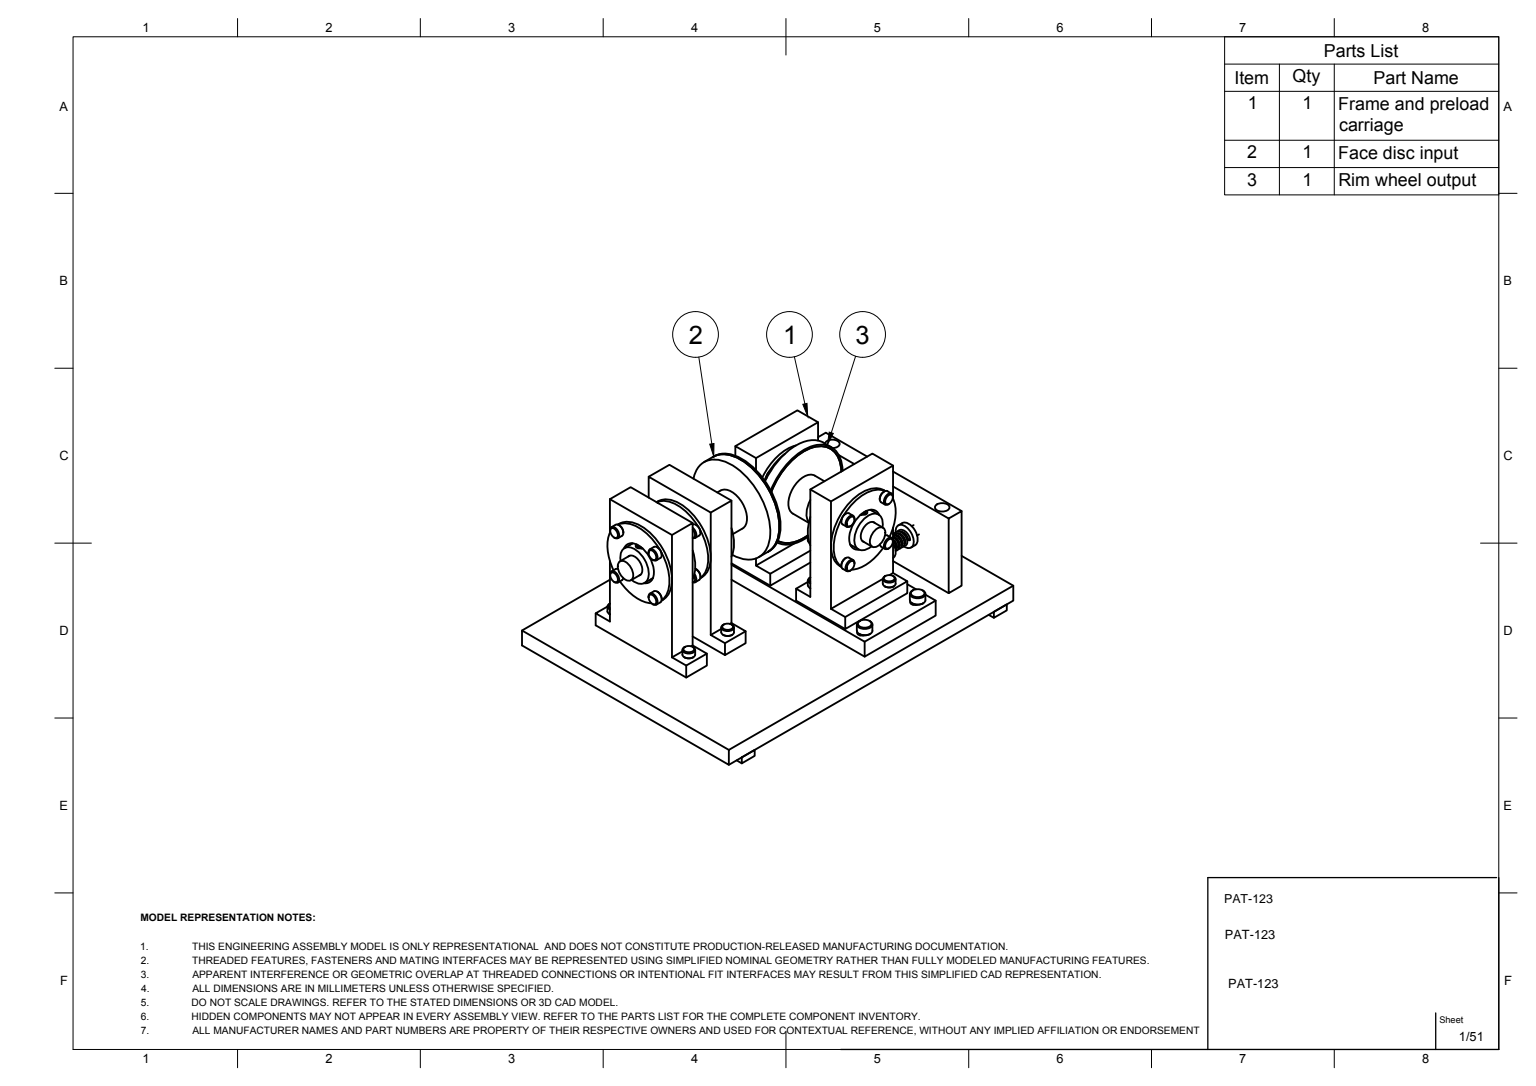
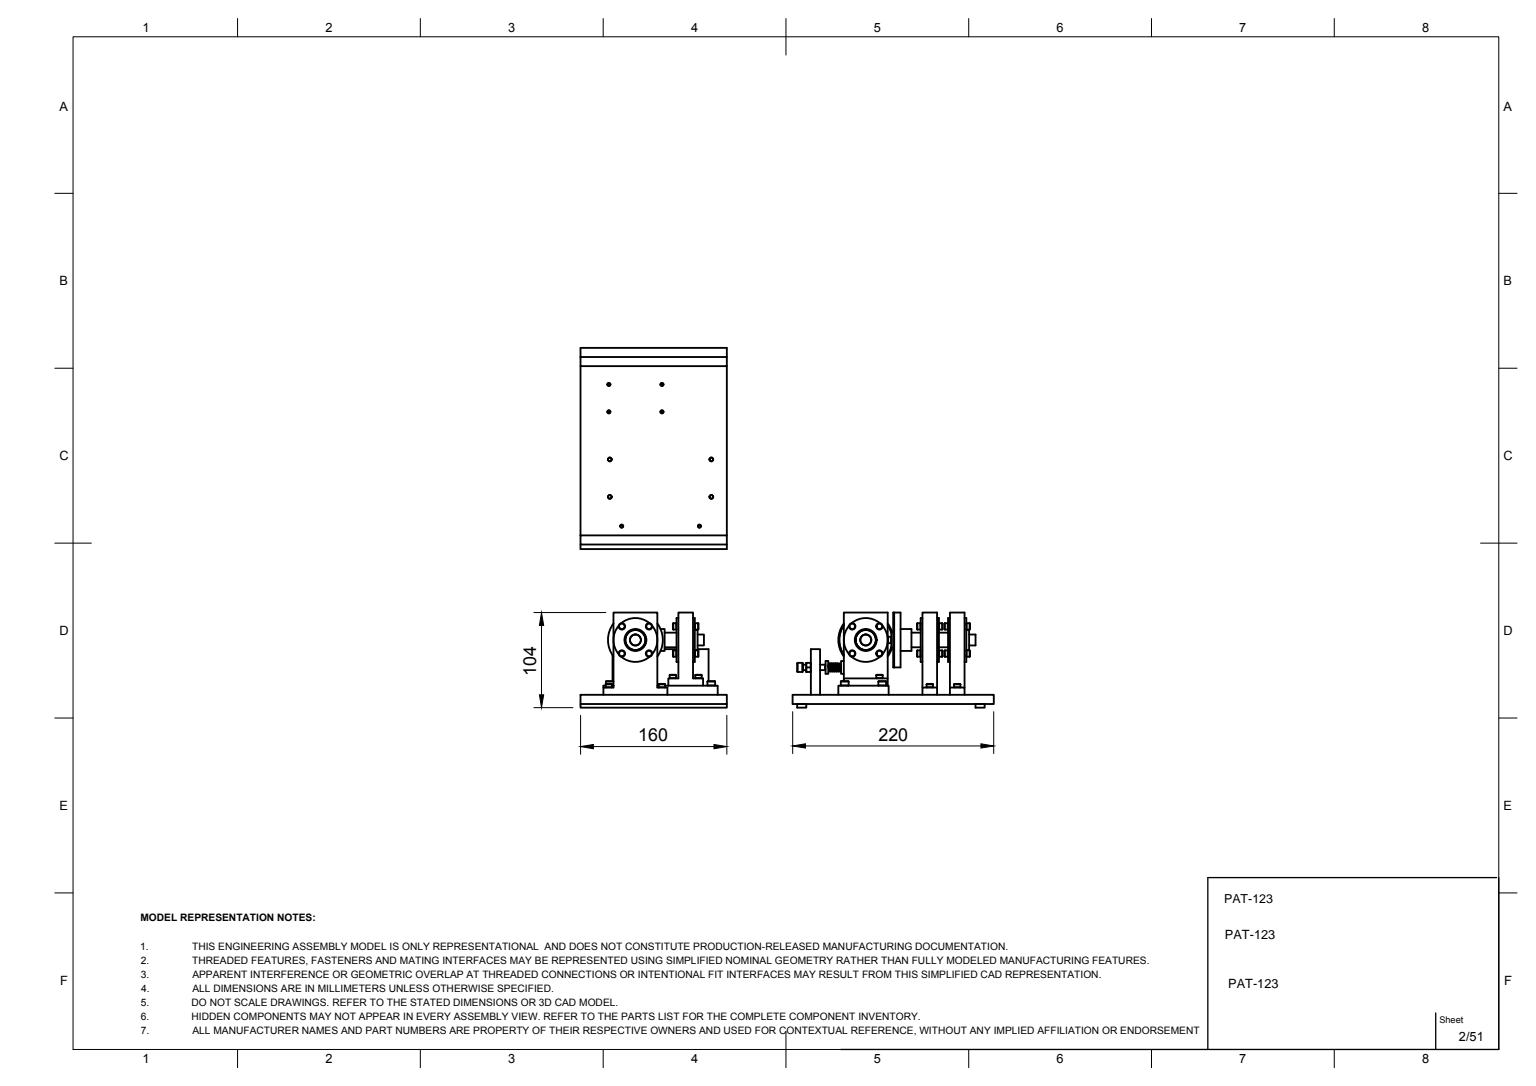
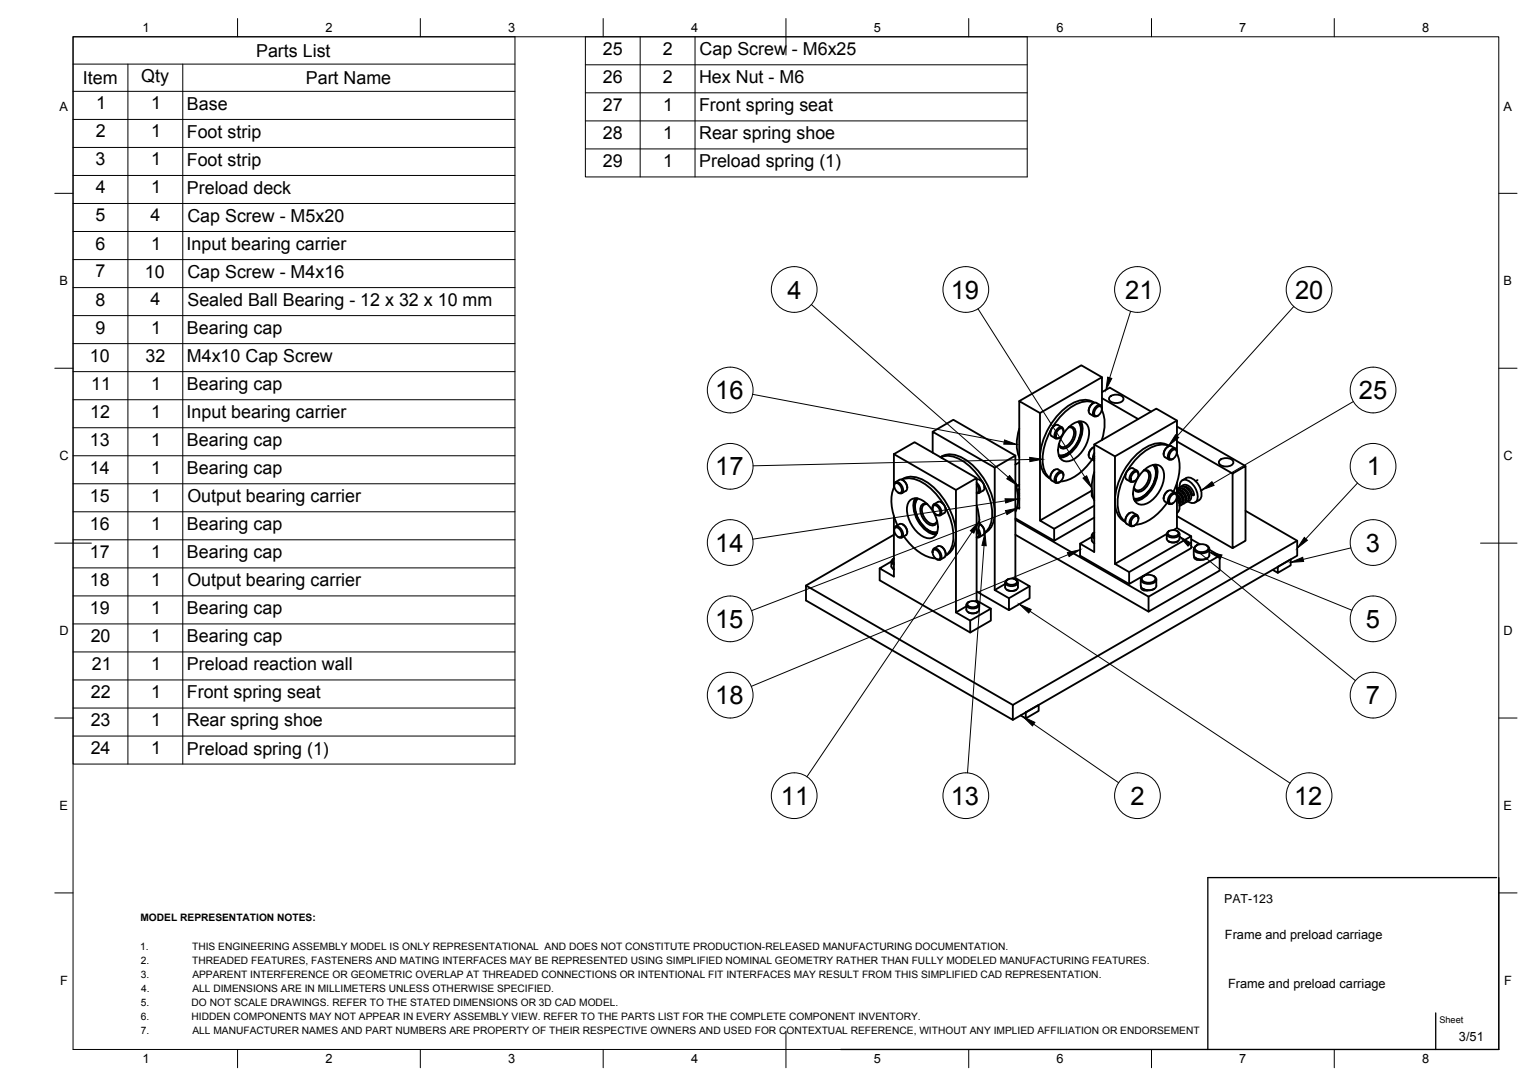
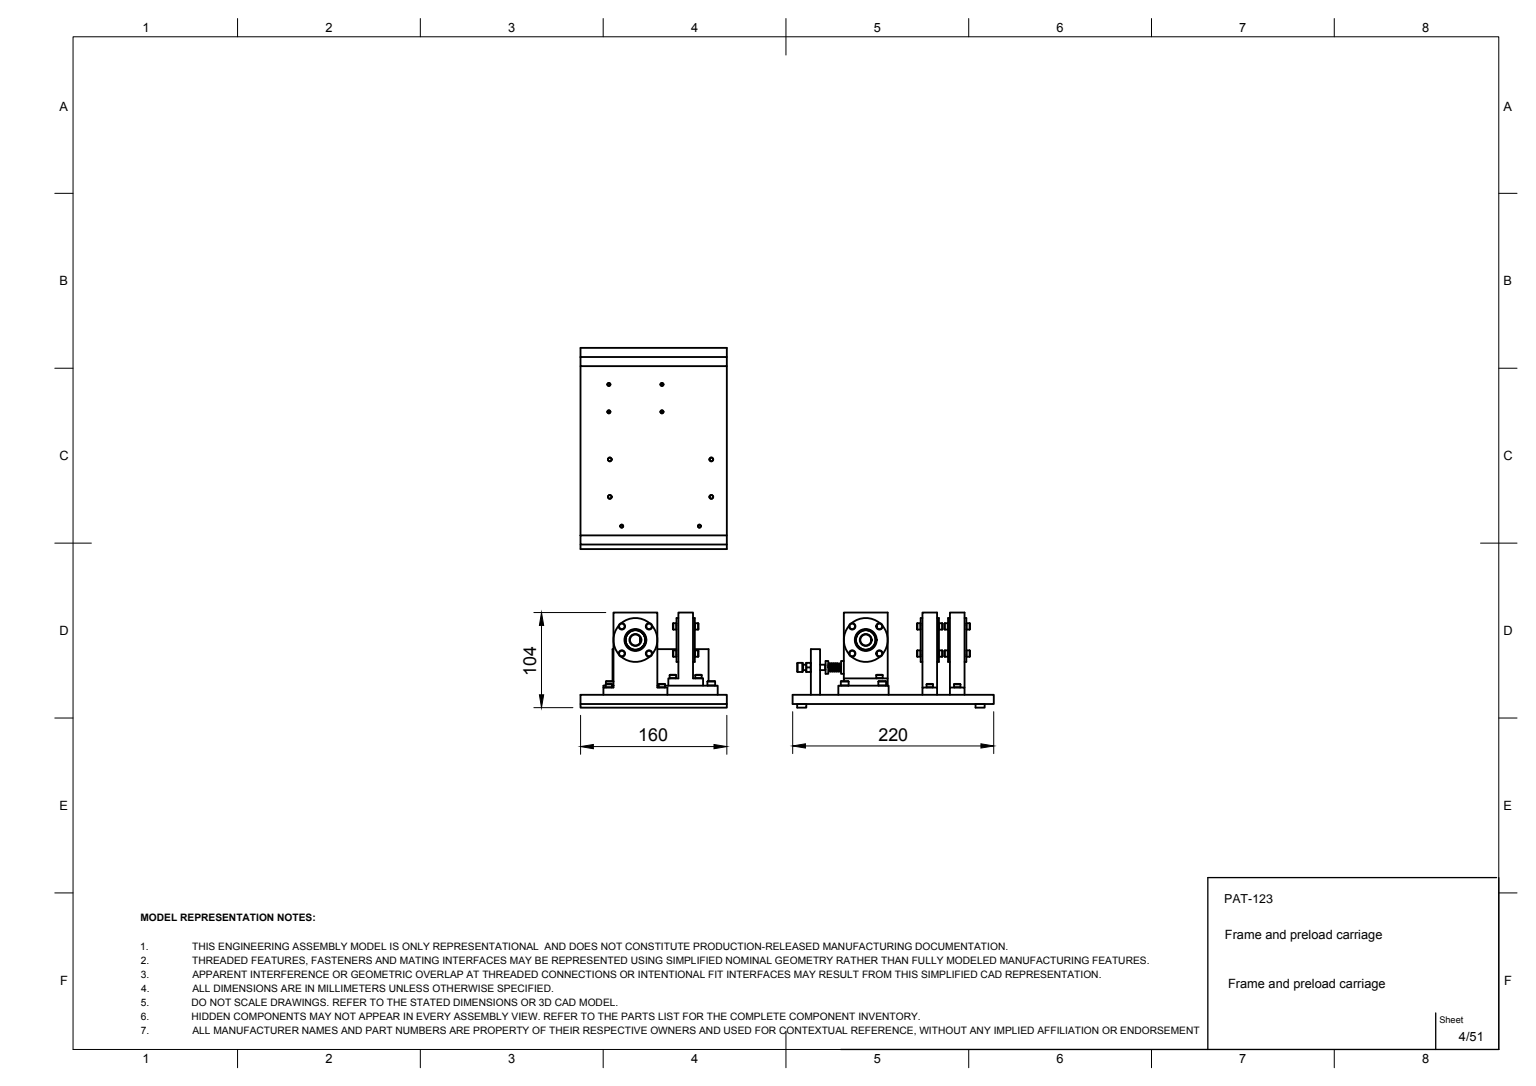
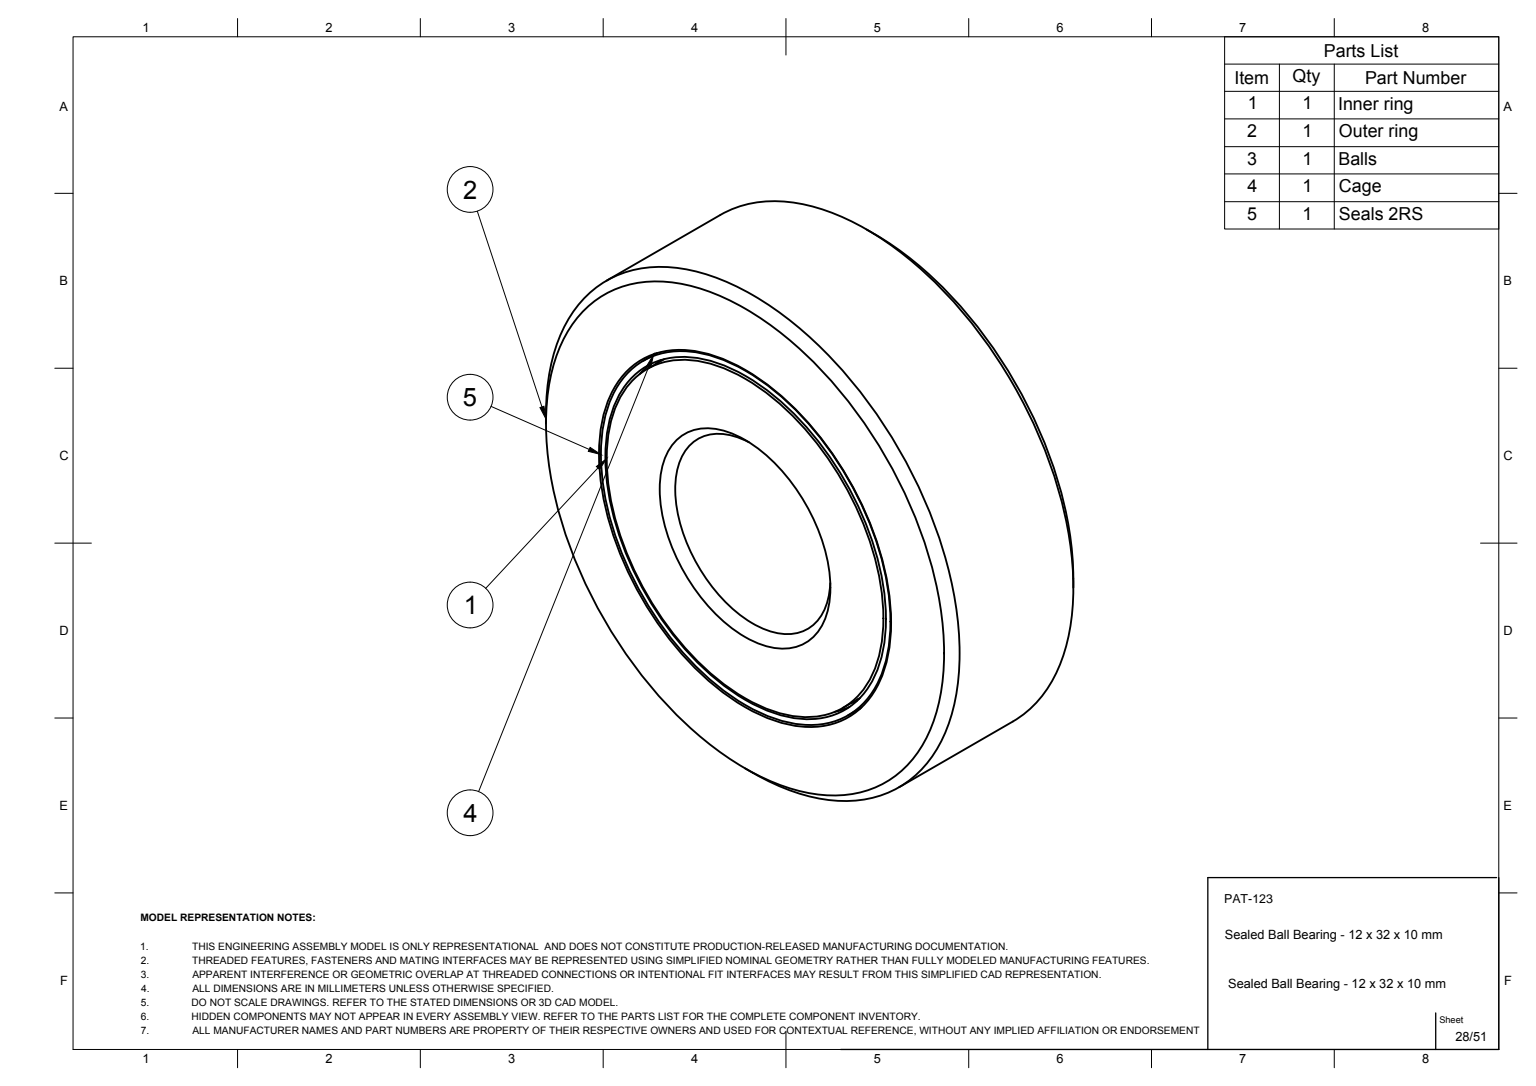
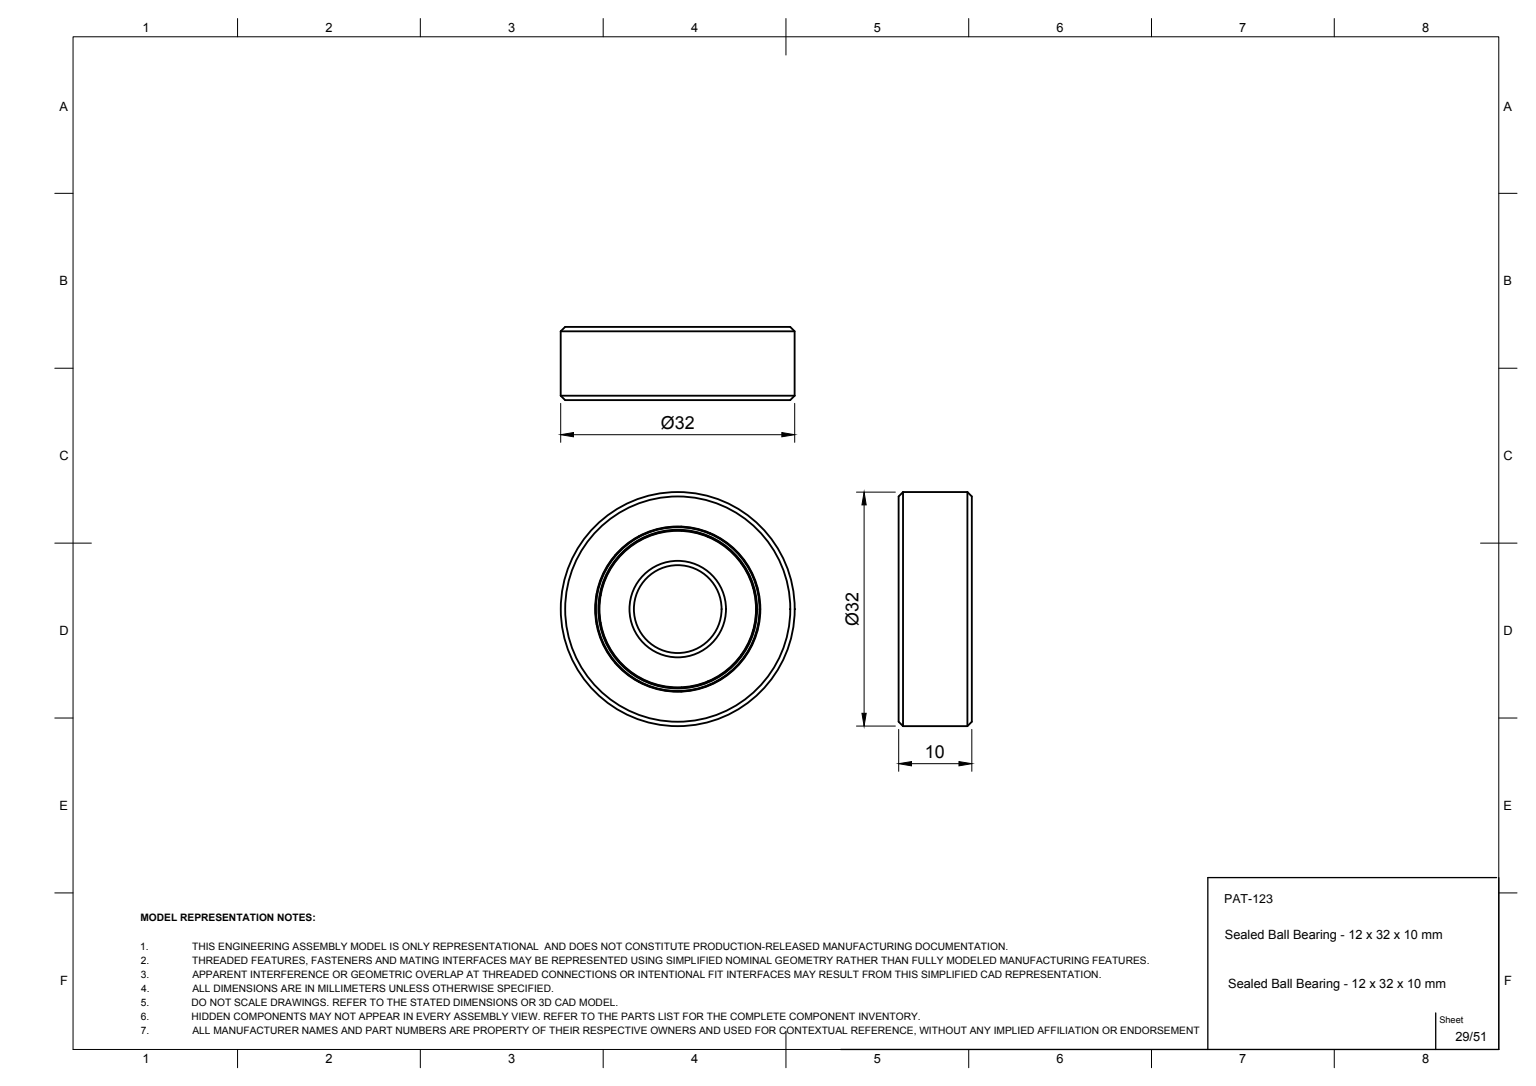
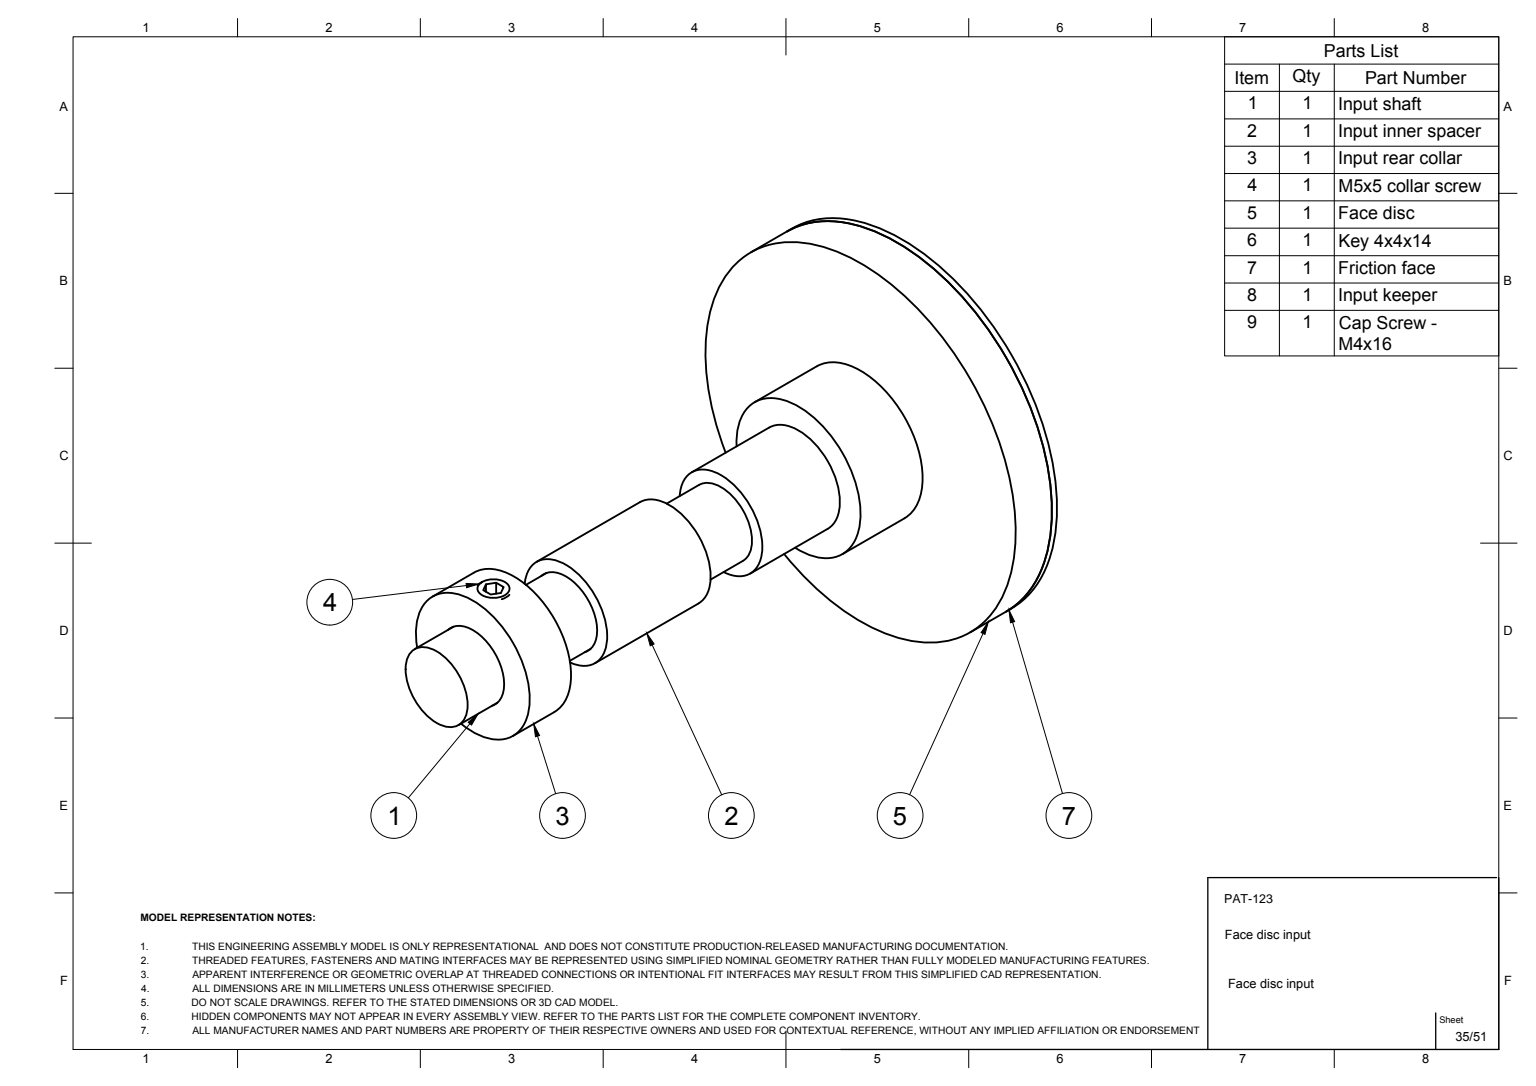
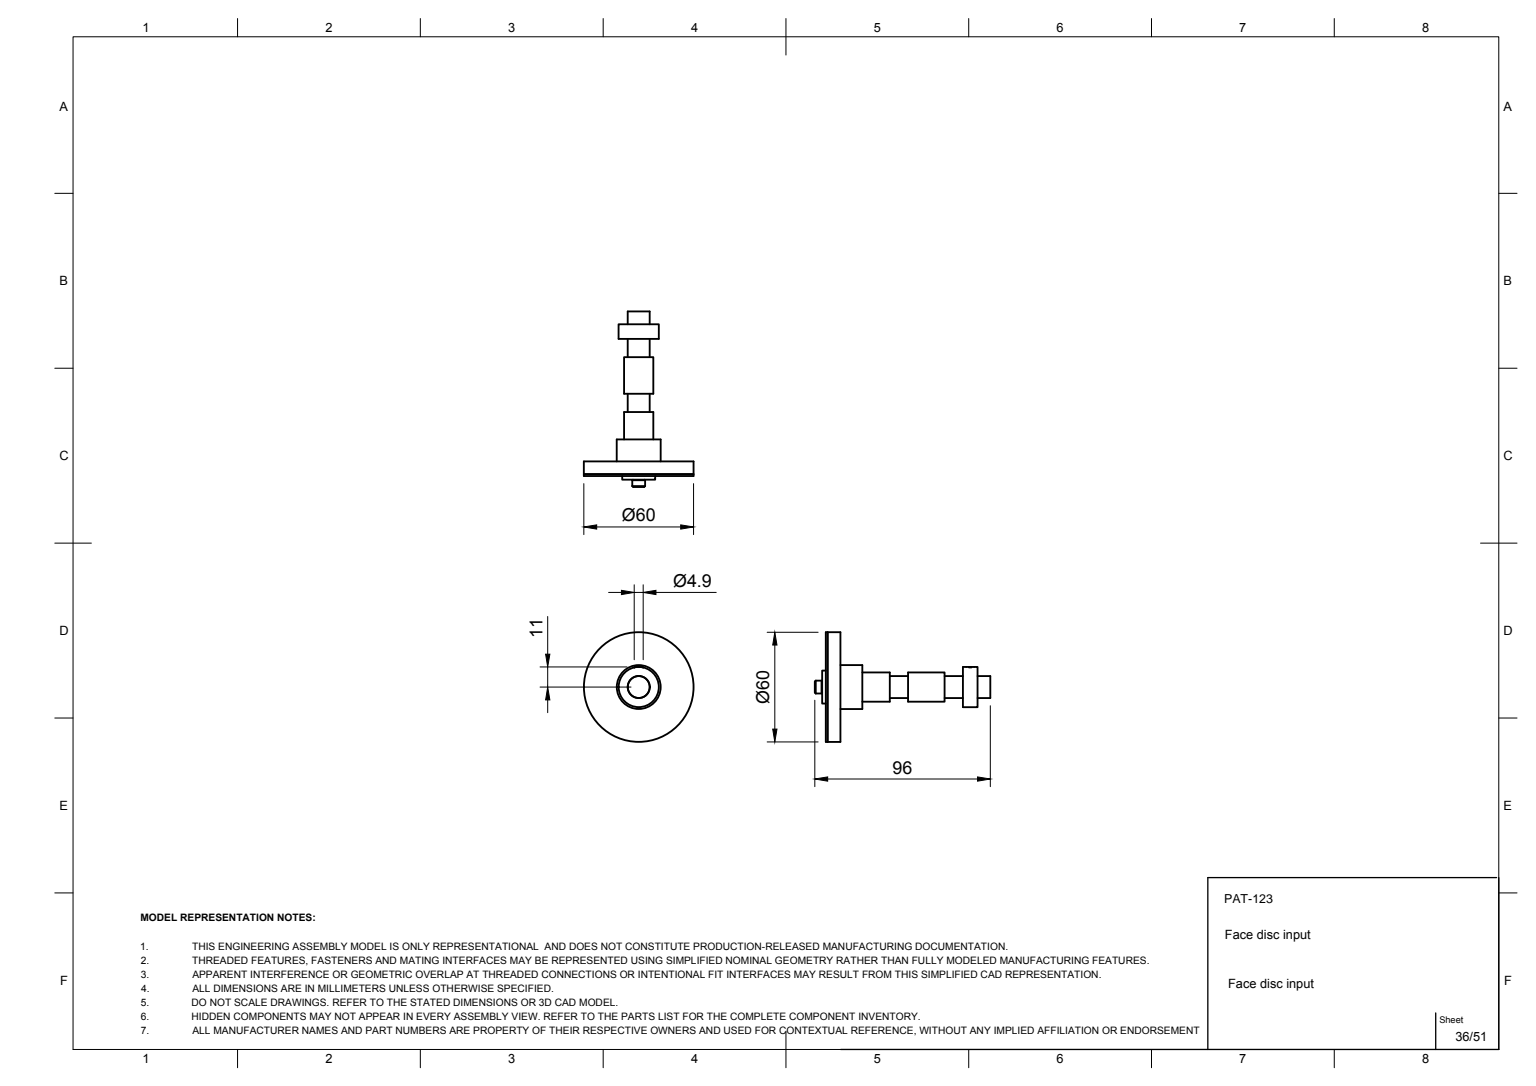
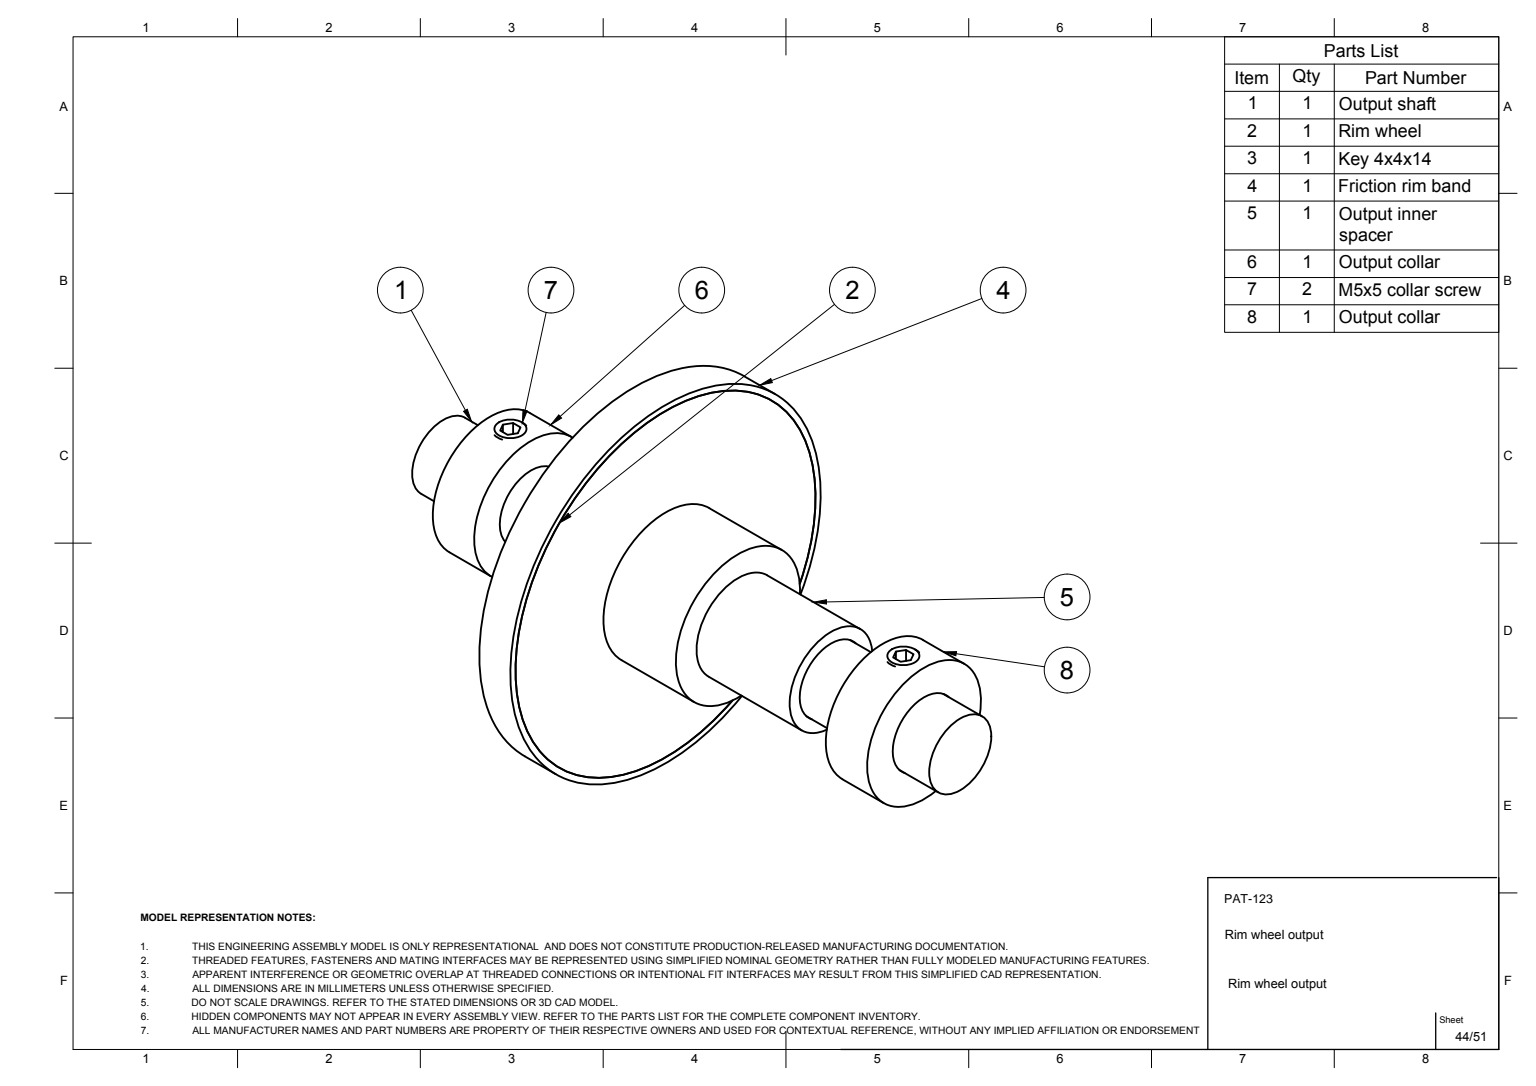
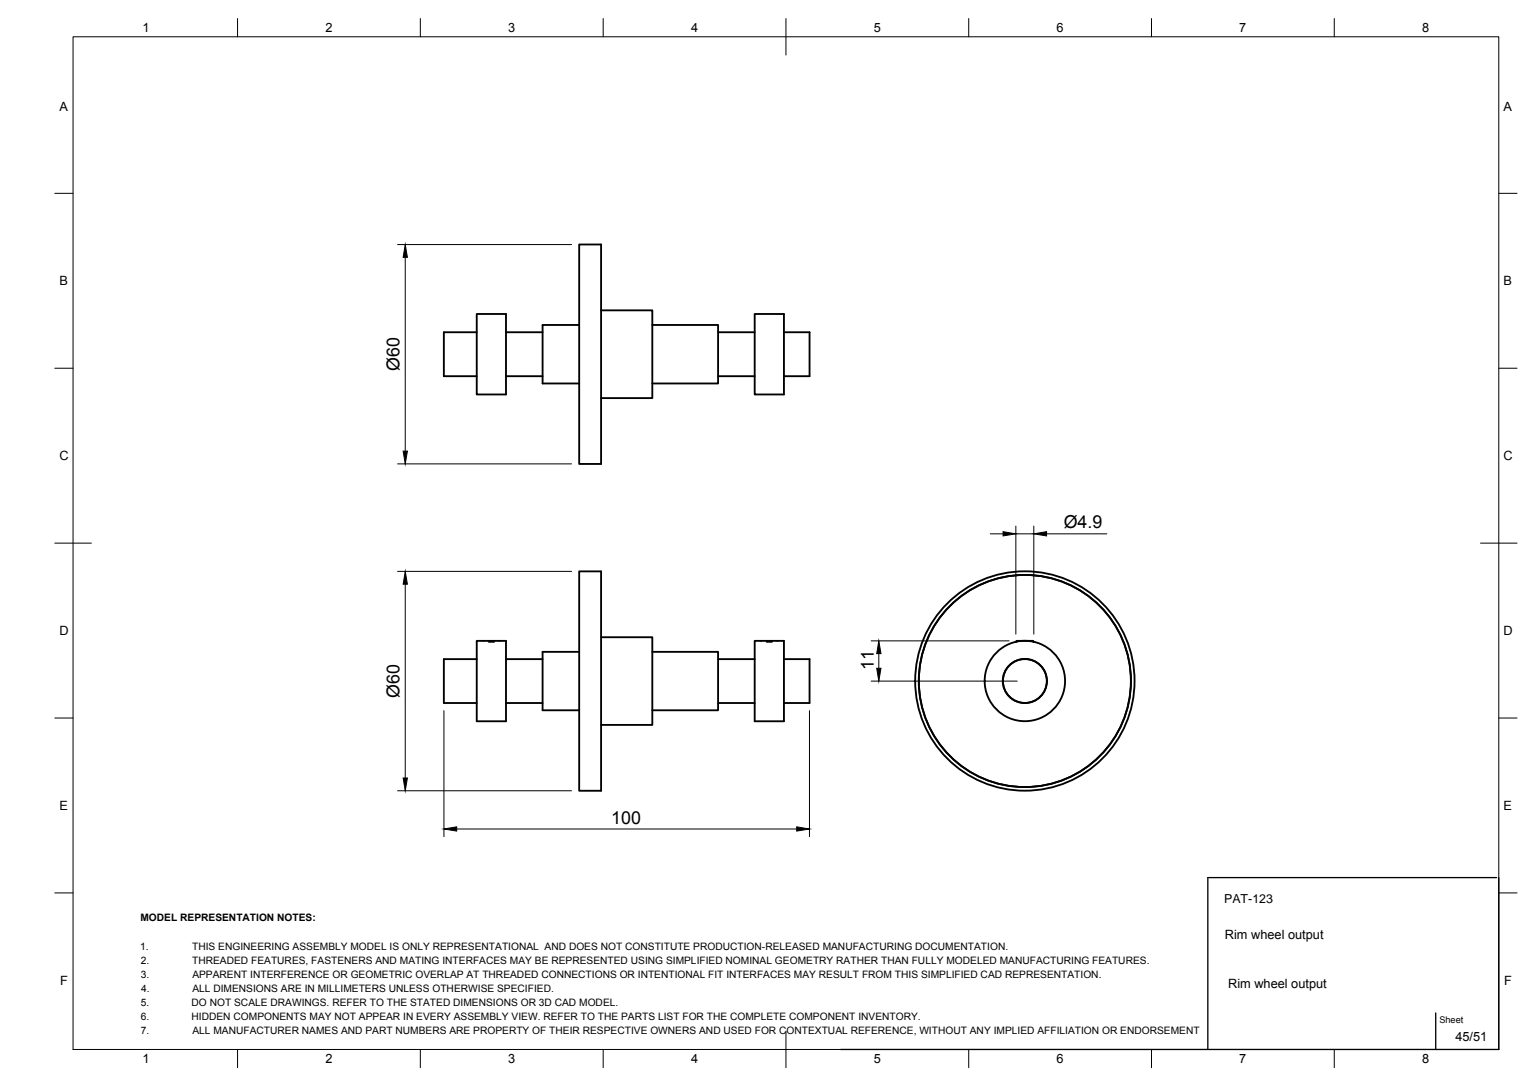
ISO-10303-21;
HEADER;
/* Generated by software containing ST-Developer
 * from STEP Tools, Inc. (www.steptools.com) 
 */

FILE_DESCRIPTION(
/* description */ ('Worm-less right-angle friction wheel drive'),
/* implementation_level */ '2;1');

FILE_NAME(
/* name */ 'PAT-123',
/* time_stamp */ '2026-10-28T03:22:36-07:00',
/* author */ (''),
/* organization */ (''),
/* preprocessor_version */ 'ST-DEVELOPER v20.2',
/* originating_system */ 'Autodesk Translation Framework v15.17.0.0',
/* authorisation */ '');

FILE_SCHEMA (('AUTOMOTIVE_DESIGN { 1 0 10303 214 3 1 1 }'));
ENDSEC;

DATA;
#10=MECHANICAL_DESIGN_GEOMETRIC_PRESENTATION_REPRESENTATION('',(#611,#612,
#613,#614,#615,#616,#617,#618,#619,#620,#621,#622,#623,#624,#625,#626,#627,
#628,#629,#630,#631,#632,#633,#634,#635,#636,#637,#638,#639,#640,#641,#642,
#643,#644,#645,#646,#647,#648,#649,#650,#651,#652,#653,#654,#655,#656,#657,
#658,#659,#660,#661,#662,#663,#664),#17046);
#11=(
BOUNDED_CURVE()
B_SPLINE_CURVE(2,(#16060,#16061,#16062),.UNSPECIFIED.,.F.,.F.)
B_SPLINE_CURVE_WITH_KNOTS((3,3),(0.144988513094728,0.791574906712449),
 .UNSPECIFIED.)
CURVE()
GEOMETRIC_REPRESENTATION_ITEM()
RATIONAL_B_SPLINE_CURVE((1.09282032302755,1.26188021535082,1.09282032302931))
REPRESENTATION_ITEM('')
);
#12=(
BOUNDED_CURVE()
B_SPLINE_CURVE(2,(#16064,#16065,#16066),.UNSPECIFIED.,.F.,.F.)
B_SPLINE_CURVE_WITH_KNOTS((3,3),(0.144988513094728,0.791574906712449),
 .UNSPECIFIED.)
CURVE()
GEOMETRIC_REPRESENTATION_ITEM()
RATIONAL_B_SPLINE_CURVE((1.09282032302755,1.26188021535082,1.09282032302931))
REPRESENTATION_ITEM('')
);
#13=(
BOUNDED_CURVE()
B_SPLINE_CURVE(2,(#16071,#16072,#16073),.UNSPECIFIED.,.F.,.F.)
B_SPLINE_CURVE_WITH_KNOTS((3,3),(0.144988513094728,0.791574906712449),
 .UNSPECIFIED.)
CURVE()
GEOMETRIC_REPRESENTATION_ITEM()
RATIONAL_B_SPLINE_CURVE((1.09282032302755,1.26188021535082,1.09282032302931))
REPRESENTATION_ITEM('')
);
#14=(
BOUNDED_CURVE()
B_SPLINE_CURVE(2,(#16075,#16076,#16077),.UNSPECIFIED.,.F.,.F.)
B_SPLINE_CURVE_WITH_KNOTS((3,3),(0.144988513094728,0.791574906712449),
 .UNSPECIFIED.)
CURVE()
GEOMETRIC_REPRESENTATION_ITEM()
RATIONAL_B_SPLINE_CURVE((1.09282032302755,1.26188021535082,1.09282032302931))
REPRESENTATION_ITEM('')
);
#15=(
BOUNDED_CURVE()
B_SPLINE_CURVE(2,(#16079,#16080,#16081),.UNSPECIFIED.,.F.,.F.)
B_SPLINE_CURVE_WITH_KNOTS((3,3),(0.144988513094728,0.791574906712449),
 .UNSPECIFIED.)
CURVE()
GEOMETRIC_REPRESENTATION_ITEM()
RATIONAL_B_SPLINE_CURVE((1.09282032302755,1.26188021535082,1.09282032302931))
REPRESENTATION_ITEM('')
);
#16=(
BOUNDED_CURVE()
B_SPLINE_CURVE(2,(#16082,#16083,#16084),.UNSPECIFIED.,.F.,.F.)
B_SPLINE_CURVE_WITH_KNOTS((3,3),(0.144988513094728,0.791574906712449),
 .UNSPECIFIED.)
CURVE()
GEOMETRIC_REPRESENTATION_ITEM()
RATIONAL_B_SPLINE_CURVE((1.09282032302755,1.26188021535082,1.09282032302931))
REPRESENTATION_ITEM('')
);
#17=(
BOUNDED_CURVE()
B_SPLINE_CURVE(2,(#16091,#16092,#16093),.UNSPECIFIED.,.F.,.F.)
B_SPLINE_CURVE_WITH_KNOTS((3,3),(0.144988513094728,0.791574906712449),
 .UNSPECIFIED.)
CURVE()
GEOMETRIC_REPRESENTATION_ITEM()
RATIONAL_B_SPLINE_CURVE((1.09282032302755,1.26188021535082,1.09282032302931))
REPRESENTATION_ITEM('')
);
#18=(
BOUNDED_CURVE()
B_SPLINE_CURVE(2,(#16095,#16096,#16097),.UNSPECIFIED.,.F.,.F.)
B_SPLINE_CURVE_WITH_KNOTS((3,3),(0.144988513094727,0.791574906712449),
 .UNSPECIFIED.)
CURVE()
GEOMETRIC_REPRESENTATION_ITEM()
RATIONAL_B_SPLINE_CURVE((1.09282032302755,1.26188021535082,1.09282032302931))
REPRESENTATION_ITEM('')
);
#19=(
BOUNDED_CURVE()
B_SPLINE_CURVE(2,(#16099,#16100,#16101),.UNSPECIFIED.,.F.,.F.)
B_SPLINE_CURVE_WITH_KNOTS((3,3),(0.144988513094728,0.791574906712449),
 .UNSPECIFIED.)
CURVE()
GEOMETRIC_REPRESENTATION_ITEM()
RATIONAL_B_SPLINE_CURVE((1.09282032302755,1.26188021535082,1.09282032302931))
REPRESENTATION_ITEM('')
);
#20=(
BOUNDED_CURVE()
B_SPLINE_CURVE(2,(#16103,#16104,#16105),.UNSPECIFIED.,.F.,.F.)
B_SPLINE_CURVE_WITH_KNOTS((3,3),(0.144988513094728,0.791574906712449),
 .UNSPECIFIED.)
CURVE()
GEOMETRIC_REPRESENTATION_ITEM()
RATIONAL_B_SPLINE_CURVE((1.09282032302755,1.26188021535082,1.09282032302931))
REPRESENTATION_ITEM('')
);
#21=(
BOUNDED_CURVE()
B_SPLINE_CURVE(2,(#16107,#16108,#16109),.UNSPECIFIED.,.F.,.F.)
B_SPLINE_CURVE_WITH_KNOTS((3,3),(0.144988513094728,0.791574906712449),
 .UNSPECIFIED.)
CURVE()
GEOMETRIC_REPRESENTATION_ITEM()
RATIONAL_B_SPLINE_CURVE((1.09282032302755,1.26188021535082,1.09282032302931))
REPRESENTATION_ITEM('')
);
#22=(
BOUNDED_CURVE()
B_SPLINE_CURVE(2,(#16110,#16111,#16112),.UNSPECIFIED.,.F.,.F.)
B_SPLINE_CURVE_WITH_KNOTS((3,3),(0.144988513094727,0.791574906712449),
 .UNSPECIFIED.)
CURVE()
GEOMETRIC_REPRESENTATION_ITEM()
RATIONAL_B_SPLINE_CURVE((1.09282032302755,1.26188021535082,1.09282032302931))
REPRESENTATION_ITEM('')
);
#23=ITEM_DEFINED_TRANSFORMATION($,$,#9262,#9384);
#24=ITEM_DEFINED_TRANSFORMATION($,$,#9282,#9385);
#25=ITEM_DEFINED_TRANSFORMATION($,$,#9302,#9386);
#26=ITEM_DEFINED_TRANSFORMATION($,$,#9317,#9387);
#27=ITEM_DEFINED_TRANSFORMATION($,$,#9367,#9388);
#28=ITEM_DEFINED_TRANSFORMATION($,$,#8744,#9565);
#29=ITEM_DEFINED_TRANSFORMATION($,$,#8781,#9566);
#30=ITEM_DEFINED_TRANSFORMATION($,$,#8788,#9567);
#31=ITEM_DEFINED_TRANSFORMATION($,$,#8795,#9568);
#32=ITEM_DEFINED_TRANSFORMATION($,$,#8846,#9569);
#33=ITEM_DEFINED_TRANSFORMATION($,$,#8878,#9570);
#34=ITEM_DEFINED_TRANSFORMATION($,$,#8903,#9571);
#35=ITEM_DEFINED_TRANSFORMATION($,$,#8928,#9572);
#36=ITEM_DEFINED_TRANSFORMATION($,$,#8960,#9573);
#37=ITEM_DEFINED_TRANSFORMATION($,$,#8985,#9574);
#38=ITEM_DEFINED_TRANSFORMATION($,$,#9010,#9575);
#39=ITEM_DEFINED_TRANSFORMATION($,$,#9042,#9576);
#40=ITEM_DEFINED_TRANSFORMATION($,$,#9067,#9577);
#41=ITEM_DEFINED_TRANSFORMATION($,$,#9092,#9578);
#42=ITEM_DEFINED_TRANSFORMATION($,$,#9124,#9579);
#43=ITEM_DEFINED_TRANSFORMATION($,$,#9149,#9580);
#44=ITEM_DEFINED_TRANSFORMATION($,$,#9174,#9581);
#45=ITEM_DEFINED_TRANSFORMATION($,$,#9201,#9582);
#46=ITEM_DEFINED_TRANSFORMATION($,$,#9207,#9583);
#47=ITEM_DEFINED_TRANSFORMATION($,$,#9213,#9584);
#48=ITEM_DEFINED_TRANSFORMATION($,$,#9218,#9585);
#49=ITEM_DEFINED_TRANSFORMATION($,$,#9224,#9586);
#50=ITEM_DEFINED_TRANSFORMATION($,$,#9230,#9587);
#51=ITEM_DEFINED_TRANSFORMATION($,$,#9235,#9588);
#52=ITEM_DEFINED_TRANSFORMATION($,$,#9235,#9589);
#53=ITEM_DEFINED_TRANSFORMATION($,$,#9235,#9590);
#54=ITEM_DEFINED_TRANSFORMATION($,$,#9235,#9591);
#55=ITEM_DEFINED_TRANSFORMATION($,$,#9539,#9592);
#56=ITEM_DEFINED_TRANSFORMATION($,$,#9539,#9593);
#57=ITEM_DEFINED_TRANSFORMATION($,$,#9261,#9594);
#58=ITEM_DEFINED_TRANSFORMATION($,$,#9389,#9595);
#59=ITEM_DEFINED_TRANSFORMATION($,$,#9389,#9596);
#60=ITEM_DEFINED_TRANSFORMATION($,$,#9389,#9597);
#61=ITEM_DEFINED_TRANSFORMATION($,$,#9389,#9598);
#62=ITEM_DEFINED_TRANSFORMATION($,$,#9389,#9599);
#63=ITEM_DEFINED_TRANSFORMATION($,$,#9389,#9600);
#64=ITEM_DEFINED_TRANSFORMATION($,$,#9389,#9601);
#65=ITEM_DEFINED_TRANSFORMATION($,$,#9389,#9602);
#66=ITEM_DEFINED_TRANSFORMATION($,$,#9539,#9603);
#67=ITEM_DEFINED_TRANSFORMATION($,$,#9539,#9604);
#68=ITEM_DEFINED_TRANSFORMATION($,$,#9261,#9605);
#69=ITEM_DEFINED_TRANSFORMATION($,$,#9389,#9606);
#70=ITEM_DEFINED_TRANSFORMATION($,$,#9389,#9607);
#71=ITEM_DEFINED_TRANSFORMATION($,$,#9389,#9608);
#72=ITEM_DEFINED_TRANSFORMATION($,$,#9389,#9609);
#73=ITEM_DEFINED_TRANSFORMATION($,$,#9389,#9610);
#74=ITEM_DEFINED_TRANSFORMATION($,$,#9389,#9611);
#75=ITEM_DEFINED_TRANSFORMATION($,$,#9389,#9612);
#76=ITEM_DEFINED_TRANSFORMATION($,$,#9389,#9613);
#77=ITEM_DEFINED_TRANSFORMATION($,$,#9539,#9614);
#78=ITEM_DEFINED_TRANSFORMATION($,$,#9539,#9615);
#79=ITEM_DEFINED_TRANSFORMATION($,$,#9261,#9616);
#80=ITEM_DEFINED_TRANSFORMATION($,$,#9389,#9617);
#81=ITEM_DEFINED_TRANSFORMATION($,$,#9389,#9618);
#82=ITEM_DEFINED_TRANSFORMATION($,$,#9389,#9619);
#83=ITEM_DEFINED_TRANSFORMATION($,$,#9389,#9620);
#84=ITEM_DEFINED_TRANSFORMATION($,$,#9389,#9621);
#85=ITEM_DEFINED_TRANSFORMATION($,$,#9389,#9622);
#86=ITEM_DEFINED_TRANSFORMATION($,$,#9389,#9623);
#87=ITEM_DEFINED_TRANSFORMATION($,$,#9389,#9624);
#88=ITEM_DEFINED_TRANSFORMATION($,$,#9539,#9625);
#89=ITEM_DEFINED_TRANSFORMATION($,$,#9539,#9626);
#90=ITEM_DEFINED_TRANSFORMATION($,$,#9261,#9627);
#91=ITEM_DEFINED_TRANSFORMATION($,$,#9389,#9628);
#92=ITEM_DEFINED_TRANSFORMATION($,$,#9389,#9629);
#93=ITEM_DEFINED_TRANSFORMATION($,$,#9389,#9630);
#94=ITEM_DEFINED_TRANSFORMATION($,$,#9389,#9631);
#95=ITEM_DEFINED_TRANSFORMATION($,$,#9389,#9632);
#96=ITEM_DEFINED_TRANSFORMATION($,$,#9389,#9633);
#97=ITEM_DEFINED_TRANSFORMATION($,$,#9389,#9634);
#98=ITEM_DEFINED_TRANSFORMATION($,$,#9389,#9635);
#99=ITEM_DEFINED_TRANSFORMATION($,$,#9539,#9636);
#100=ITEM_DEFINED_TRANSFORMATION($,$,#9539,#9637);
#101=ITEM_DEFINED_TRANSFORMATION($,$,#9413,#9638);
#102=ITEM_DEFINED_TRANSFORMATION($,$,#9439,#9639);
#103=ITEM_DEFINED_TRANSFORMATION($,$,#9413,#9640);
#104=ITEM_DEFINED_TRANSFORMATION($,$,#9439,#9641);
#105=ITEM_DEFINED_TRANSFORMATION($,$,#9456,#9752);
#106=ITEM_DEFINED_TRANSFORMATION($,$,#9481,#9753);
#107=ITEM_DEFINED_TRANSFORMATION($,$,#9490,#9754);
#108=ITEM_DEFINED_TRANSFORMATION($,$,#9505,#9755);
#109=ITEM_DEFINED_TRANSFORMATION($,$,#9521,#9756);
#110=ITEM_DEFINED_TRANSFORMATION($,$,#9530,#9757);
#111=ITEM_DEFINED_TRANSFORMATION($,$,#9737,#9758);
#112=ITEM_DEFINED_TRANSFORMATION($,$,#9726,#9759);
#113=ITEM_DEFINED_TRANSFORMATION($,$,#9539,#9760);
#114=ITEM_DEFINED_TRANSFORMATION($,$,#9643,#9761);
#115=ITEM_DEFINED_TRANSFORMATION($,$,#9664,#9762);
#116=ITEM_DEFINED_TRANSFORMATION($,$,#9680,#9763);
#117=ITEM_DEFINED_TRANSFORMATION($,$,#9689,#9764);
#118=ITEM_DEFINED_TRANSFORMATION($,$,#9698,#9765);
#119=ITEM_DEFINED_TRANSFORMATION($,$,#9712,#9766);
#120=ITEM_DEFINED_TRANSFORMATION($,$,#9726,#9767);
#121=ITEM_DEFINED_TRANSFORMATION($,$,#9737,#9768);
#122=ITEM_DEFINED_TRANSFORMATION($,$,#9737,#9769);
#123=ITEM_DEFINED_TRANSFORMATION($,$,#8743,#9770);
#124=ITEM_DEFINED_TRANSFORMATION($,$,#9455,#9771);
#125=ITEM_DEFINED_TRANSFORMATION($,$,#9642,#9772);
#126=(
REPRESENTATION_RELATIONSHIP($,$,#17285,#17284)
REPRESENTATION_RELATIONSHIP_WITH_TRANSFORMATION(#23)
SHAPE_REPRESENTATION_RELATIONSHIP()
);
#127=(
REPRESENTATION_RELATIONSHIP($,$,#17286,#17284)
REPRESENTATION_RELATIONSHIP_WITH_TRANSFORMATION(#24)
SHAPE_REPRESENTATION_RELATIONSHIP()
);
#128=(
REPRESENTATION_RELATIONSHIP($,$,#17287,#17284)
REPRESENTATION_RELATIONSHIP_WITH_TRANSFORMATION(#25)
SHAPE_REPRESENTATION_RELATIONSHIP()
);
#129=(
REPRESENTATION_RELATIONSHIP($,$,#17288,#17284)
REPRESENTATION_RELATIONSHIP_WITH_TRANSFORMATION(#26)
SHAPE_REPRESENTATION_RELATIONSHIP()
);
#130=(
REPRESENTATION_RELATIONSHIP($,$,#17289,#17284)
REPRESENTATION_RELATIONSHIP_WITH_TRANSFORMATION(#27)
SHAPE_REPRESENTATION_RELATIONSHIP()
);
#131=(
REPRESENTATION_RELATIONSHIP($,$,#17260,#17259)
REPRESENTATION_RELATIONSHIP_WITH_TRANSFORMATION(#28)
SHAPE_REPRESENTATION_RELATIONSHIP()
);
#132=(
REPRESENTATION_RELATIONSHIP($,$,#17261,#17259)
REPRESENTATION_RELATIONSHIP_WITH_TRANSFORMATION(#29)
SHAPE_REPRESENTATION_RELATIONSHIP()
);
#133=(
REPRESENTATION_RELATIONSHIP($,$,#17262,#17259)
REPRESENTATION_RELATIONSHIP_WITH_TRANSFORMATION(#30)
SHAPE_REPRESENTATION_RELATIONSHIP()
);
#134=(
REPRESENTATION_RELATIONSHIP($,$,#17263,#17259)
REPRESENTATION_RELATIONSHIP_WITH_TRANSFORMATION(#31)
SHAPE_REPRESENTATION_RELATIONSHIP()
);
#135=(
REPRESENTATION_RELATIONSHIP($,$,#17264,#17259)
REPRESENTATION_RELATIONSHIP_WITH_TRANSFORMATION(#32)
SHAPE_REPRESENTATION_RELATIONSHIP()
);
#136=(
REPRESENTATION_RELATIONSHIP($,$,#17265,#17259)
REPRESENTATION_RELATIONSHIP_WITH_TRANSFORMATION(#33)
SHAPE_REPRESENTATION_RELATIONSHIP()
);
#137=(
REPRESENTATION_RELATIONSHIP($,$,#17266,#17259)
REPRESENTATION_RELATIONSHIP_WITH_TRANSFORMATION(#34)
SHAPE_REPRESENTATION_RELATIONSHIP()
);
#138=(
REPRESENTATION_RELATIONSHIP($,$,#17267,#17259)
REPRESENTATION_RELATIONSHIP_WITH_TRANSFORMATION(#35)
SHAPE_REPRESENTATION_RELATIONSHIP()
);
#139=(
REPRESENTATION_RELATIONSHIP($,$,#17268,#17259)
REPRESENTATION_RELATIONSHIP_WITH_TRANSFORMATION(#36)
SHAPE_REPRESENTATION_RELATIONSHIP()
);
#140=(
REPRESENTATION_RELATIONSHIP($,$,#17269,#17259)
REPRESENTATION_RELATIONSHIP_WITH_TRANSFORMATION(#37)
SHAPE_REPRESENTATION_RELATIONSHIP()
);
#141=(
REPRESENTATION_RELATIONSHIP($,$,#17270,#17259)
REPRESENTATION_RELATIONSHIP_WITH_TRANSFORMATION(#38)
SHAPE_REPRESENTATION_RELATIONSHIP()
);
#142=(
REPRESENTATION_RELATIONSHIP($,$,#17271,#17259)
REPRESENTATION_RELATIONSHIP_WITH_TRANSFORMATION(#39)
SHAPE_REPRESENTATION_RELATIONSHIP()
);
#143=(
REPRESENTATION_RELATIONSHIP($,$,#17272,#17259)
REPRESENTATION_RELATIONSHIP_WITH_TRANSFORMATION(#40)
SHAPE_REPRESENTATION_RELATIONSHIP()
);
#144=(
REPRESENTATION_RELATIONSHIP($,$,#17273,#17259)
REPRESENTATION_RELATIONSHIP_WITH_TRANSFORMATION(#41)
SHAPE_REPRESENTATION_RELATIONSHIP()
);
#145=(
REPRESENTATION_RELATIONSHIP($,$,#17274,#17259)
REPRESENTATION_RELATIONSHIP_WITH_TRANSFORMATION(#42)
SHAPE_REPRESENTATION_RELATIONSHIP()
);
#146=(
REPRESENTATION_RELATIONSHIP($,$,#17275,#17259)
REPRESENTATION_RELATIONSHIP_WITH_TRANSFORMATION(#43)
SHAPE_REPRESENTATION_RELATIONSHIP()
);
#147=(
REPRESENTATION_RELATIONSHIP($,$,#17276,#17259)
REPRESENTATION_RELATIONSHIP_WITH_TRANSFORMATION(#44)
SHAPE_REPRESENTATION_RELATIONSHIP()
);
#148=(
REPRESENTATION_RELATIONSHIP($,$,#17277,#17259)
REPRESENTATION_RELATIONSHIP_WITH_TRANSFORMATION(#45)
SHAPE_REPRESENTATION_RELATIONSHIP()
);
#149=(
REPRESENTATION_RELATIONSHIP($,$,#17278,#17259)
REPRESENTATION_RELATIONSHIP_WITH_TRANSFORMATION(#46)
SHAPE_REPRESENTATION_RELATIONSHIP()
);
#150=(
REPRESENTATION_RELATIONSHIP($,$,#17279,#17259)
REPRESENTATION_RELATIONSHIP_WITH_TRANSFORMATION(#47)
SHAPE_REPRESENTATION_RELATIONSHIP()
);
#151=(
REPRESENTATION_RELATIONSHIP($,$,#17280,#17259)
REPRESENTATION_RELATIONSHIP_WITH_TRANSFORMATION(#48)
SHAPE_REPRESENTATION_RELATIONSHIP()
);
#152=(
REPRESENTATION_RELATIONSHIP($,$,#17281,#17259)
REPRESENTATION_RELATIONSHIP_WITH_TRANSFORMATION(#49)
SHAPE_REPRESENTATION_RELATIONSHIP()
);
#153=(
REPRESENTATION_RELATIONSHIP($,$,#17282,#17259)
REPRESENTATION_RELATIONSHIP_WITH_TRANSFORMATION(#50)
SHAPE_REPRESENTATION_RELATIONSHIP()
);
#154=(
REPRESENTATION_RELATIONSHIP($,$,#17283,#17259)
REPRESENTATION_RELATIONSHIP_WITH_TRANSFORMATION(#51)
SHAPE_REPRESENTATION_RELATIONSHIP()
);
#155=(
REPRESENTATION_RELATIONSHIP($,$,#17283,#17259)
REPRESENTATION_RELATIONSHIP_WITH_TRANSFORMATION(#52)
SHAPE_REPRESENTATION_RELATIONSHIP()
);
#156=(
REPRESENTATION_RELATIONSHIP($,$,#17283,#17259)
REPRESENTATION_RELATIONSHIP_WITH_TRANSFORMATION(#53)
SHAPE_REPRESENTATION_RELATIONSHIP()
);
#157=(
REPRESENTATION_RELATIONSHIP($,$,#17283,#17259)
REPRESENTATION_RELATIONSHIP_WITH_TRANSFORMATION(#54)
SHAPE_REPRESENTATION_RELATIONSHIP()
);
#158=(
REPRESENTATION_RELATIONSHIP($,$,#17300,#17259)
REPRESENTATION_RELATIONSHIP_WITH_TRANSFORMATION(#55)
SHAPE_REPRESENTATION_RELATIONSHIP()
);
#159=(
REPRESENTATION_RELATIONSHIP($,$,#17300,#17259)
REPRESENTATION_RELATIONSHIP_WITH_TRANSFORMATION(#56)
SHAPE_REPRESENTATION_RELATIONSHIP()
);
#160=(
REPRESENTATION_RELATIONSHIP($,$,#17284,#17259)
REPRESENTATION_RELATIONSHIP_WITH_TRANSFORMATION(#57)
SHAPE_REPRESENTATION_RELATIONSHIP()
);
#161=(
REPRESENTATION_RELATIONSHIP($,$,#17290,#17259)
REPRESENTATION_RELATIONSHIP_WITH_TRANSFORMATION(#58)
SHAPE_REPRESENTATION_RELATIONSHIP()
);
#162=(
REPRESENTATION_RELATIONSHIP($,$,#17290,#17259)
REPRESENTATION_RELATIONSHIP_WITH_TRANSFORMATION(#59)
SHAPE_REPRESENTATION_RELATIONSHIP()
);
#163=(
REPRESENTATION_RELATIONSHIP($,$,#17290,#17259)
REPRESENTATION_RELATIONSHIP_WITH_TRANSFORMATION(#60)
SHAPE_REPRESENTATION_RELATIONSHIP()
);
#164=(
REPRESENTATION_RELATIONSHIP($,$,#17290,#17259)
REPRESENTATION_RELATIONSHIP_WITH_TRANSFORMATION(#61)
SHAPE_REPRESENTATION_RELATIONSHIP()
);
#165=(
REPRESENTATION_RELATIONSHIP($,$,#17290,#17259)
REPRESENTATION_RELATIONSHIP_WITH_TRANSFORMATION(#62)
SHAPE_REPRESENTATION_RELATIONSHIP()
);
#166=(
REPRESENTATION_RELATIONSHIP($,$,#17290,#17259)
REPRESENTATION_RELATIONSHIP_WITH_TRANSFORMATION(#63)
SHAPE_REPRESENTATION_RELATIONSHIP()
);
#167=(
REPRESENTATION_RELATIONSHIP($,$,#17290,#17259)
REPRESENTATION_RELATIONSHIP_WITH_TRANSFORMATION(#64)
SHAPE_REPRESENTATION_RELATIONSHIP()
);
#168=(
REPRESENTATION_RELATIONSHIP($,$,#17290,#17259)
REPRESENTATION_RELATIONSHIP_WITH_TRANSFORMATION(#65)
SHAPE_REPRESENTATION_RELATIONSHIP()
);
#169=(
REPRESENTATION_RELATIONSHIP($,$,#17300,#17259)
REPRESENTATION_RELATIONSHIP_WITH_TRANSFORMATION(#66)
SHAPE_REPRESENTATION_RELATIONSHIP()
);
#170=(
REPRESENTATION_RELATIONSHIP($,$,#17300,#17259)
REPRESENTATION_RELATIONSHIP_WITH_TRANSFORMATION(#67)
SHAPE_REPRESENTATION_RELATIONSHIP()
);
#171=(
REPRESENTATION_RELATIONSHIP($,$,#17284,#17259)
REPRESENTATION_RELATIONSHIP_WITH_TRANSFORMATION(#68)
SHAPE_REPRESENTATION_RELATIONSHIP()
);
#172=(
REPRESENTATION_RELATIONSHIP($,$,#17290,#17259)
REPRESENTATION_RELATIONSHIP_WITH_TRANSFORMATION(#69)
SHAPE_REPRESENTATION_RELATIONSHIP()
);
#173=(
REPRESENTATION_RELATIONSHIP($,$,#17290,#17259)
REPRESENTATION_RELATIONSHIP_WITH_TRANSFORMATION(#70)
SHAPE_REPRESENTATION_RELATIONSHIP()
);
#174=(
REPRESENTATION_RELATIONSHIP($,$,#17290,#17259)
REPRESENTATION_RELATIONSHIP_WITH_TRANSFORMATION(#71)
SHAPE_REPRESENTATION_RELATIONSHIP()
);
#175=(
REPRESENTATION_RELATIONSHIP($,$,#17290,#17259)
REPRESENTATION_RELATIONSHIP_WITH_TRANSFORMATION(#72)
SHAPE_REPRESENTATION_RELATIONSHIP()
);
#176=(
REPRESENTATION_RELATIONSHIP($,$,#17290,#17259)
REPRESENTATION_RELATIONSHIP_WITH_TRANSFORMATION(#73)
SHAPE_REPRESENTATION_RELATIONSHIP()
);
#177=(
REPRESENTATION_RELATIONSHIP($,$,#17290,#17259)
REPRESENTATION_RELATIONSHIP_WITH_TRANSFORMATION(#74)
SHAPE_REPRESENTATION_RELATIONSHIP()
);
#178=(
REPRESENTATION_RELATIONSHIP($,$,#17290,#17259)
REPRESENTATION_RELATIONSHIP_WITH_TRANSFORMATION(#75)
SHAPE_REPRESENTATION_RELATIONSHIP()
);
#179=(
REPRESENTATION_RELATIONSHIP($,$,#17290,#17259)
REPRESENTATION_RELATIONSHIP_WITH_TRANSFORMATION(#76)
SHAPE_REPRESENTATION_RELATIONSHIP()
);
#180=(
REPRESENTATION_RELATIONSHIP($,$,#17300,#17259)
REPRESENTATION_RELATIONSHIP_WITH_TRANSFORMATION(#77)
SHAPE_REPRESENTATION_RELATIONSHIP()
);
#181=(
REPRESENTATION_RELATIONSHIP($,$,#17300,#17259)
REPRESENTATION_RELATIONSHIP_WITH_TRANSFORMATION(#78)
SHAPE_REPRESENTATION_RELATIONSHIP()
);
#182=(
REPRESENTATION_RELATIONSHIP($,$,#17284,#17259)
REPRESENTATION_RELATIONSHIP_WITH_TRANSFORMATION(#79)
SHAPE_REPRESENTATION_RELATIONSHIP()
);
#183=(
REPRESENTATION_RELATIONSHIP($,$,#17290,#17259)
REPRESENTATION_RELATIONSHIP_WITH_TRANSFORMATION(#80)
SHAPE_REPRESENTATION_RELATIONSHIP()
);
#184=(
REPRESENTATION_RELATIONSHIP($,$,#17290,#17259)
REPRESENTATION_RELATIONSHIP_WITH_TRANSFORMATION(#81)
SHAPE_REPRESENTATION_RELATIONSHIP()
);
#185=(
REPRESENTATION_RELATIONSHIP($,$,#17290,#17259)
REPRESENTATION_RELATIONSHIP_WITH_TRANSFORMATION(#82)
SHAPE_REPRESENTATION_RELATIONSHIP()
);
#186=(
REPRESENTATION_RELATIONSHIP($,$,#17290,#17259)
REPRESENTATION_RELATIONSHIP_WITH_TRANSFORMATION(#83)
SHAPE_REPRESENTATION_RELATIONSHIP()
);
#187=(
REPRESENTATION_RELATIONSHIP($,$,#17290,#17259)
REPRESENTATION_RELATIONSHIP_WITH_TRANSFORMATION(#84)
SHAPE_REPRESENTATION_RELATIONSHIP()
);
#188=(
REPRESENTATION_RELATIONSHIP($,$,#17290,#17259)
REPRESENTATION_RELATIONSHIP_WITH_TRANSFORMATION(#85)
SHAPE_REPRESENTATION_RELATIONSHIP()
);
#189=(
REPRESENTATION_RELATIONSHIP($,$,#17290,#17259)
REPRESENTATION_RELATIONSHIP_WITH_TRANSFORMATION(#86)
SHAPE_REPRESENTATION_RELATIONSHIP()
);
#190=(
REPRESENTATION_RELATIONSHIP($,$,#17290,#17259)
REPRESENTATION_RELATIONSHIP_WITH_TRANSFORMATION(#87)
SHAPE_REPRESENTATION_RELATIONSHIP()
);
#191=(
REPRESENTATION_RELATIONSHIP($,$,#17300,#17259)
REPRESENTATION_RELATIONSHIP_WITH_TRANSFORMATION(#88)
SHAPE_REPRESENTATION_RELATIONSHIP()
);
#192=(
REPRESENTATION_RELATIONSHIP($,$,#17300,#17259)
REPRESENTATION_RELATIONSHIP_WITH_TRANSFORMATION(#89)
SHAPE_REPRESENTATION_RELATIONSHIP()
);
#193=(
REPRESENTATION_RELATIONSHIP($,$,#17284,#17259)
REPRESENTATION_RELATIONSHIP_WITH_TRANSFORMATION(#90)
SHAPE_REPRESENTATION_RELATIONSHIP()
);
#194=(
REPRESENTATION_RELATIONSHIP($,$,#17290,#17259)
REPRESENTATION_RELATIONSHIP_WITH_TRANSFORMATION(#91)
SHAPE_REPRESENTATION_RELATIONSHIP()
);
#195=(
REPRESENTATION_RELATIONSHIP($,$,#17290,#17259)
REPRESENTATION_RELATIONSHIP_WITH_TRANSFORMATION(#92)
SHAPE_REPRESENTATION_RELATIONSHIP()
);
#196=(
REPRESENTATION_RELATIONSHIP($,$,#17290,#17259)
REPRESENTATION_RELATIONSHIP_WITH_TRANSFORMATION(#93)
SHAPE_REPRESENTATION_RELATIONSHIP()
);
#197=(
REPRESENTATION_RELATIONSHIP($,$,#17290,#17259)
REPRESENTATION_RELATIONSHIP_WITH_TRANSFORMATION(#94)
SHAPE_REPRESENTATION_RELATIONSHIP()
);
#198=(
REPRESENTATION_RELATIONSHIP($,$,#17290,#17259)
REPRESENTATION_RELATIONSHIP_WITH_TRANSFORMATION(#95)
SHAPE_REPRESENTATION_RELATIONSHIP()
);
#199=(
REPRESENTATION_RELATIONSHIP($,$,#17290,#17259)
REPRESENTATION_RELATIONSHIP_WITH_TRANSFORMATION(#96)
SHAPE_REPRESENTATION_RELATIONSHIP()
);
#200=(
REPRESENTATION_RELATIONSHIP($,$,#17290,#17259)
REPRESENTATION_RELATIONSHIP_WITH_TRANSFORMATION(#97)
SHAPE_REPRESENTATION_RELATIONSHIP()
);
#201=(
REPRESENTATION_RELATIONSHIP($,$,#17290,#17259)
REPRESENTATION_RELATIONSHIP_WITH_TRANSFORMATION(#98)
SHAPE_REPRESENTATION_RELATIONSHIP()
);
#202=(
REPRESENTATION_RELATIONSHIP($,$,#17300,#17259)
REPRESENTATION_RELATIONSHIP_WITH_TRANSFORMATION(#99)
SHAPE_REPRESENTATION_RELATIONSHIP()
);
#203=(
REPRESENTATION_RELATIONSHIP($,$,#17300,#17259)
REPRESENTATION_RELATIONSHIP_WITH_TRANSFORMATION(#100)
SHAPE_REPRESENTATION_RELATIONSHIP()
);
#204=(
REPRESENTATION_RELATIONSHIP($,$,#17291,#17259)
REPRESENTATION_RELATIONSHIP_WITH_TRANSFORMATION(#101)
SHAPE_REPRESENTATION_RELATIONSHIP()
);
#205=(
REPRESENTATION_RELATIONSHIP($,$,#17292,#17259)
REPRESENTATION_RELATIONSHIP_WITH_TRANSFORMATION(#102)
SHAPE_REPRESENTATION_RELATIONSHIP()
);
#206=(
REPRESENTATION_RELATIONSHIP($,$,#17291,#17259)
REPRESENTATION_RELATIONSHIP_WITH_TRANSFORMATION(#103)
SHAPE_REPRESENTATION_RELATIONSHIP()
);
#207=(
REPRESENTATION_RELATIONSHIP($,$,#17292,#17259)
REPRESENTATION_RELATIONSHIP_WITH_TRANSFORMATION(#104)
SHAPE_REPRESENTATION_RELATIONSHIP()
);
#208=(
REPRESENTATION_RELATIONSHIP($,$,#17294,#17293)
REPRESENTATION_RELATIONSHIP_WITH_TRANSFORMATION(#105)
SHAPE_REPRESENTATION_RELATIONSHIP()
);
#209=(
REPRESENTATION_RELATIONSHIP($,$,#17295,#17293)
REPRESENTATION_RELATIONSHIP_WITH_TRANSFORMATION(#106)
SHAPE_REPRESENTATION_RELATIONSHIP()
);
#210=(
REPRESENTATION_RELATIONSHIP($,$,#17296,#17293)
REPRESENTATION_RELATIONSHIP_WITH_TRANSFORMATION(#107)
SHAPE_REPRESENTATION_RELATIONSHIP()
);
#211=(
REPRESENTATION_RELATIONSHIP($,$,#17297,#17293)
REPRESENTATION_RELATIONSHIP_WITH_TRANSFORMATION(#108)
SHAPE_REPRESENTATION_RELATIONSHIP()
);
#212=(
REPRESENTATION_RELATIONSHIP($,$,#17298,#17293)
REPRESENTATION_RELATIONSHIP_WITH_TRANSFORMATION(#109)
SHAPE_REPRESENTATION_RELATIONSHIP()
);
#213=(
REPRESENTATION_RELATIONSHIP($,$,#17299,#17293)
REPRESENTATION_RELATIONSHIP_WITH_TRANSFORMATION(#110)
SHAPE_REPRESENTATION_RELATIONSHIP()
);
#214=(
REPRESENTATION_RELATIONSHIP($,$,#17309,#17293)
REPRESENTATION_RELATIONSHIP_WITH_TRANSFORMATION(#111)
SHAPE_REPRESENTATION_RELATIONSHIP()
);
#215=(
REPRESENTATION_RELATIONSHIP($,$,#17308,#17293)
REPRESENTATION_RELATIONSHIP_WITH_TRANSFORMATION(#112)
SHAPE_REPRESENTATION_RELATIONSHIP()
);
#216=(
REPRESENTATION_RELATIONSHIP($,$,#17300,#17293)
REPRESENTATION_RELATIONSHIP_WITH_TRANSFORMATION(#113)
SHAPE_REPRESENTATION_RELATIONSHIP()
);
#217=(
REPRESENTATION_RELATIONSHIP($,$,#17302,#17301)
REPRESENTATION_RELATIONSHIP_WITH_TRANSFORMATION(#114)
SHAPE_REPRESENTATION_RELATIONSHIP()
);
#218=(
REPRESENTATION_RELATIONSHIP($,$,#17303,#17301)
REPRESENTATION_RELATIONSHIP_WITH_TRANSFORMATION(#115)
SHAPE_REPRESENTATION_RELATIONSHIP()
);
#219=(
REPRESENTATION_RELATIONSHIP($,$,#17304,#17301)
REPRESENTATION_RELATIONSHIP_WITH_TRANSFORMATION(#116)
SHAPE_REPRESENTATION_RELATIONSHIP()
);
#220=(
REPRESENTATION_RELATIONSHIP($,$,#17305,#17301)
REPRESENTATION_RELATIONSHIP_WITH_TRANSFORMATION(#117)
SHAPE_REPRESENTATION_RELATIONSHIP()
);
#221=(
REPRESENTATION_RELATIONSHIP($,$,#17306,#17301)
REPRESENTATION_RELATIONSHIP_WITH_TRANSFORMATION(#118)
SHAPE_REPRESENTATION_RELATIONSHIP()
);
#222=(
REPRESENTATION_RELATIONSHIP($,$,#17307,#17301)
REPRESENTATION_RELATIONSHIP_WITH_TRANSFORMATION(#119)
SHAPE_REPRESENTATION_RELATIONSHIP()
);
#223=(
REPRESENTATION_RELATIONSHIP($,$,#17308,#17301)
REPRESENTATION_RELATIONSHIP_WITH_TRANSFORMATION(#120)
SHAPE_REPRESENTATION_RELATIONSHIP()
);
#224=(
REPRESENTATION_RELATIONSHIP($,$,#17309,#17301)
REPRESENTATION_RELATIONSHIP_WITH_TRANSFORMATION(#121)
SHAPE_REPRESENTATION_RELATIONSHIP()
);
#225=(
REPRESENTATION_RELATIONSHIP($,$,#17309,#17301)
REPRESENTATION_RELATIONSHIP_WITH_TRANSFORMATION(#122)
SHAPE_REPRESENTATION_RELATIONSHIP()
);
#226=(
REPRESENTATION_RELATIONSHIP($,$,#17259,#17258)
REPRESENTATION_RELATIONSHIP_WITH_TRANSFORMATION(#123)
SHAPE_REPRESENTATION_RELATIONSHIP()
);
#227=(
REPRESENTATION_RELATIONSHIP($,$,#17293,#17258)
REPRESENTATION_RELATIONSHIP_WITH_TRANSFORMATION(#124)
SHAPE_REPRESENTATION_RELATIONSHIP()
);
#228=(
REPRESENTATION_RELATIONSHIP($,$,#17301,#17258)
REPRESENTATION_RELATIONSHIP_WITH_TRANSFORMATION(#125)
SHAPE_REPRESENTATION_RELATIONSHIP()
);
#229=CONTEXT_DEPENDENT_SHAPE_REPRESENTATION(#126,#17135);
#230=CONTEXT_DEPENDENT_SHAPE_REPRESENTATION(#127,#17136);
#231=CONTEXT_DEPENDENT_SHAPE_REPRESENTATION(#128,#17137);
#232=CONTEXT_DEPENDENT_SHAPE_REPRESENTATION(#129,#17138);
#233=CONTEXT_DEPENDENT_SHAPE_REPRESENTATION(#130,#17139);
#234=CONTEXT_DEPENDENT_SHAPE_REPRESENTATION(#131,#17151);
#235=CONTEXT_DEPENDENT_SHAPE_REPRESENTATION(#132,#17152);
#236=CONTEXT_DEPENDENT_SHAPE_REPRESENTATION(#133,#17153);
#237=CONTEXT_DEPENDENT_SHAPE_REPRESENTATION(#134,#17154);
#238=CONTEXT_DEPENDENT_SHAPE_REPRESENTATION(#135,#17155);
#239=CONTEXT_DEPENDENT_SHAPE_REPRESENTATION(#136,#17156);
#240=CONTEXT_DEPENDENT_SHAPE_REPRESENTATION(#137,#17157);
#241=CONTEXT_DEPENDENT_SHAPE_REPRESENTATION(#138,#17158);
#242=CONTEXT_DEPENDENT_SHAPE_REPRESENTATION(#139,#17159);
#243=CONTEXT_DEPENDENT_SHAPE_REPRESENTATION(#140,#17160);
#244=CONTEXT_DEPENDENT_SHAPE_REPRESENTATION(#141,#17161);
#245=CONTEXT_DEPENDENT_SHAPE_REPRESENTATION(#142,#17162);
#246=CONTEXT_DEPENDENT_SHAPE_REPRESENTATION(#143,#17163);
#247=CONTEXT_DEPENDENT_SHAPE_REPRESENTATION(#144,#17164);
#248=CONTEXT_DEPENDENT_SHAPE_REPRESENTATION(#145,#17165);
#249=CONTEXT_DEPENDENT_SHAPE_REPRESENTATION(#146,#17166);
#250=CONTEXT_DEPENDENT_SHAPE_REPRESENTATION(#147,#17167);
#251=CONTEXT_DEPENDENT_SHAPE_REPRESENTATION(#148,#17168);
#252=CONTEXT_DEPENDENT_SHAPE_REPRESENTATION(#149,#17169);
#253=CONTEXT_DEPENDENT_SHAPE_REPRESENTATION(#150,#17170);
#254=CONTEXT_DEPENDENT_SHAPE_REPRESENTATION(#151,#17171);
#255=CONTEXT_DEPENDENT_SHAPE_REPRESENTATION(#152,#17172);
#256=CONTEXT_DEPENDENT_SHAPE_REPRESENTATION(#153,#17173);
#257=CONTEXT_DEPENDENT_SHAPE_REPRESENTATION(#154,#17174);
#258=CONTEXT_DEPENDENT_SHAPE_REPRESENTATION(#155,#17175);
#259=CONTEXT_DEPENDENT_SHAPE_REPRESENTATION(#156,#17176);
#260=CONTEXT_DEPENDENT_SHAPE_REPRESENTATION(#157,#17177);
#261=CONTEXT_DEPENDENT_SHAPE_REPRESENTATION(#158,#17178);
#262=CONTEXT_DEPENDENT_SHAPE_REPRESENTATION(#159,#17179);
#263=CONTEXT_DEPENDENT_SHAPE_REPRESENTATION(#160,#17180);
#264=CONTEXT_DEPENDENT_SHAPE_REPRESENTATION(#161,#17181);
#265=CONTEXT_DEPENDENT_SHAPE_REPRESENTATION(#162,#17182);
#266=CONTEXT_DEPENDENT_SHAPE_REPRESENTATION(#163,#17183);
#267=CONTEXT_DEPENDENT_SHAPE_REPRESENTATION(#164,#17184);
#268=CONTEXT_DEPENDENT_SHAPE_REPRESENTATION(#165,#17185);
#269=CONTEXT_DEPENDENT_SHAPE_REPRESENTATION(#166,#17186);
#270=CONTEXT_DEPENDENT_SHAPE_REPRESENTATION(#167,#17187);
#271=CONTEXT_DEPENDENT_SHAPE_REPRESENTATION(#168,#17188);
#272=CONTEXT_DEPENDENT_SHAPE_REPRESENTATION(#169,#17189);
#273=CONTEXT_DEPENDENT_SHAPE_REPRESENTATION(#170,#17190);
#274=CONTEXT_DEPENDENT_SHAPE_REPRESENTATION(#171,#17191);
#275=CONTEXT_DEPENDENT_SHAPE_REPRESENTATION(#172,#17192);
#276=CONTEXT_DEPENDENT_SHAPE_REPRESENTATION(#173,#17193);
#277=CONTEXT_DEPENDENT_SHAPE_REPRESENTATION(#174,#17194);
#278=CONTEXT_DEPENDENT_SHAPE_REPRESENTATION(#175,#17195);
#279=CONTEXT_DEPENDENT_SHAPE_REPRESENTATION(#176,#17196);
#280=CONTEXT_DEPENDENT_SHAPE_REPRESENTATION(#177,#17197);
#281=CONTEXT_DEPENDENT_SHAPE_REPRESENTATION(#178,#17198);
#282=CONTEXT_DEPENDENT_SHAPE_REPRESENTATION(#179,#17199);
#283=CONTEXT_DEPENDENT_SHAPE_REPRESENTATION(#180,#17200);
#284=CONTEXT_DEPENDENT_SHAPE_REPRESENTATION(#181,#17201);
#285=CONTEXT_DEPENDENT_SHAPE_REPRESENTATION(#182,#17202);
#286=CONTEXT_DEPENDENT_SHAPE_REPRESENTATION(#183,#17203);
#287=CONTEXT_DEPENDENT_SHAPE_REPRESENTATION(#184,#17204);
#288=CONTEXT_DEPENDENT_SHAPE_REPRESENTATION(#185,#17205);
#289=CONTEXT_DEPENDENT_SHAPE_REPRESENTATION(#186,#17206);
#290=CONTEXT_DEPENDENT_SHAPE_REPRESENTATION(#187,#17207);
#291=CONTEXT_DEPENDENT_SHAPE_REPRESENTATION(#188,#17208);
#292=CONTEXT_DEPENDENT_SHAPE_REPRESENTATION(#189,#17209);
#293=CONTEXT_DEPENDENT_SHAPE_REPRESENTATION(#190,#17210);
#294=CONTEXT_DEPENDENT_SHAPE_REPRESENTATION(#191,#17211);
#295=CONTEXT_DEPENDENT_SHAPE_REPRESENTATION(#192,#17212);
#296=CONTEXT_DEPENDENT_SHAPE_REPRESENTATION(#193,#17213);
#297=CONTEXT_DEPENDENT_SHAPE_REPRESENTATION(#194,#17214);
#298=CONTEXT_DEPENDENT_SHAPE_REPRESENTATION(#195,#17215);
#299=CONTEXT_DEPENDENT_SHAPE_REPRESENTATION(#196,#17216);
#300=CONTEXT_DEPENDENT_SHAPE_REPRESENTATION(#197,#17217);
#301=CONTEXT_DEPENDENT_SHAPE_REPRESENTATION(#198,#17218);
#302=CONTEXT_DEPENDENT_SHAPE_REPRESENTATION(#199,#17219);
#303=CONTEXT_DEPENDENT_SHAPE_REPRESENTATION(#200,#17220);
#304=CONTEXT_DEPENDENT_SHAPE_REPRESENTATION(#201,#17221);
#305=CONTEXT_DEPENDENT_SHAPE_REPRESENTATION(#202,#17222);
#306=CONTEXT_DEPENDENT_SHAPE_REPRESENTATION(#203,#17223);
#307=CONTEXT_DEPENDENT_SHAPE_REPRESENTATION(#204,#17224);
#308=CONTEXT_DEPENDENT_SHAPE_REPRESENTATION(#205,#17225);
#309=CONTEXT_DEPENDENT_SHAPE_REPRESENTATION(#206,#17226);
#310=CONTEXT_DEPENDENT_SHAPE_REPRESENTATION(#207,#17227);
#311=CONTEXT_DEPENDENT_SHAPE_REPRESENTATION(#208,#17237);
#312=CONTEXT_DEPENDENT_SHAPE_REPRESENTATION(#209,#17238);
#313=CONTEXT_DEPENDENT_SHAPE_REPRESENTATION(#210,#17239);
#314=CONTEXT_DEPENDENT_SHAPE_REPRESENTATION(#211,#17240);
#315=CONTEXT_DEPENDENT_SHAPE_REPRESENTATION(#212,#17241);
#316=CONTEXT_DEPENDENT_SHAPE_REPRESENTATION(#213,#17242);
#317=CONTEXT_DEPENDENT_SHAPE_REPRESENTATION(#214,#17243);
#318=CONTEXT_DEPENDENT_SHAPE_REPRESENTATION(#215,#17244);
#319=CONTEXT_DEPENDENT_SHAPE_REPRESENTATION(#216,#17245);
#320=CONTEXT_DEPENDENT_SHAPE_REPRESENTATION(#217,#17246);
#321=CONTEXT_DEPENDENT_SHAPE_REPRESENTATION(#218,#17247);
#322=CONTEXT_DEPENDENT_SHAPE_REPRESENTATION(#219,#17248);
#323=CONTEXT_DEPENDENT_SHAPE_REPRESENTATION(#220,#17249);
#324=CONTEXT_DEPENDENT_SHAPE_REPRESENTATION(#221,#17250);
#325=CONTEXT_DEPENDENT_SHAPE_REPRESENTATION(#222,#17251);
#326=CONTEXT_DEPENDENT_SHAPE_REPRESENTATION(#223,#17252);
#327=CONTEXT_DEPENDENT_SHAPE_REPRESENTATION(#224,#17253);
#328=CONTEXT_DEPENDENT_SHAPE_REPRESENTATION(#225,#17254);
#329=CONTEXT_DEPENDENT_SHAPE_REPRESENTATION(#226,#17255);
#330=CONTEXT_DEPENDENT_SHAPE_REPRESENTATION(#227,#17256);
#331=CONTEXT_DEPENDENT_SHAPE_REPRESENTATION(#228,#17257);
#332=NEXT_ASSEMBLY_USAGE_OCCURRENCE('Inner ring:1','Inner ring:1',
'Inner ring:1',#17337,#17338,'Inner ring:1');
#333=NEXT_ASSEMBLY_USAGE_OCCURRENCE('Outer ring:1','Outer ring:1',
'Outer ring:1',#17337,#17339,'Outer ring:1');
#334=NEXT_ASSEMBLY_USAGE_OCCURRENCE('Balls:1','Balls:1','Balls:1',#17337,
#17340,'Balls:1');
#335=NEXT_ASSEMBLY_USAGE_OCCURRENCE('Cage:1','Cage:1','Cage:1',#17337,#17341,
'Cage:1');
#336=NEXT_ASSEMBLY_USAGE_OCCURRENCE('Seals 2RS:1','Seals 2RS:1',
'Seals 2RS:1',#17337,#17342,'Seals 2RS:1');
#337=NEXT_ASSEMBLY_USAGE_OCCURRENCE('Base:1','Base:1','Base:1',#17312,#17313,
'Base:1');
#338=NEXT_ASSEMBLY_USAGE_OCCURRENCE('Foot strip:1','Foot strip:1',
'Foot strip:1',#17312,#17314,'Foot strip:1');
#339=NEXT_ASSEMBLY_USAGE_OCCURRENCE('Foot strip (1):1',
'Foot strip (1):1','Foot strip (1):1',#17312,#17315,'Foot strip (1):1');
#340=NEXT_ASSEMBLY_USAGE_OCCURRENCE('Preload deck:1','Preload deck:1',
'Preload deck:1',#17312,#17316,'Preload deck:1');
#341=NEXT_ASSEMBLY_USAGE_OCCURRENCE('Input bearing carrier:1',
'Input bearing carrier:1','Input bearing carrier:1',#17312,#17317,
'Input bearing carrier:1');
#342=NEXT_ASSEMBLY_USAGE_OCCURRENCE('Bearing cap:1','Bearing cap:1',
'Bearing cap:1',#17312,#17318,'Bearing cap:1');
#343=NEXT_ASSEMBLY_USAGE_OCCURRENCE('Bearing cap (1):1',
'Bearing cap (1):1','Bearing cap (1):1',#17312,#17319,
'Bearing cap (1):1');
#344=NEXT_ASSEMBLY_USAGE_OCCURRENCE('Input bearing carrier (1):1',
'Input bearing carrier (1):1','Input bearing carrier (1):1',#17312,#17320,
'Input bearing carrier (1):1');
#345=NEXT_ASSEMBLY_USAGE_OCCURRENCE('Bearing cap (2):1',
'Bearing cap (2):1','Bearing cap (2):1',#17312,#17321,
'Bearing cap (2):1');
#346=NEXT_ASSEMBLY_USAGE_OCCURRENCE('Bearing cap (3):1',
'Bearing cap (3):1','Bearing cap (3):1',#17312,#17322,
'Bearing cap (3):1');
#347=NEXT_ASSEMBLY_USAGE_OCCURRENCE('Output bearing carrier:1',
'Output bearing carrier:1','Output bearing carrier:1',#17312,#17323,
'Output bearing carrier:1');
#348=NEXT_ASSEMBLY_USAGE_OCCURRENCE('Bearing cap (4):1',
'Bearing cap (4):1','Bearing cap (4):1',#17312,#17324,
'Bearing cap (4):1');
#349=NEXT_ASSEMBLY_USAGE_OCCURRENCE('Bearing cap (5):1',
'Bearing cap (5):1','Bearing cap (5):1',#17312,#17325,
'Bearing cap (5):1');
#350=NEXT_ASSEMBLY_USAGE_OCCURRENCE('Output bearing carrier (1):1',
'Output bearing carrier (1):1','Output bearing carrier (1):1',#17312,#17326,
'Output bearing carrier (1):1');
#351=NEXT_ASSEMBLY_USAGE_OCCURRENCE('Bearing cap (6):1',
'Bearing cap (6):1','Bearing cap (6):1',#17312,#17327,
'Bearing cap (6):1');
#352=NEXT_ASSEMBLY_USAGE_OCCURRENCE('Bearing cap (7):1',
'Bearing cap (7):1','Bearing cap (7):1',#17312,#17328,
'Bearing cap (7):1');
#353=NEXT_ASSEMBLY_USAGE_OCCURRENCE('Preload reaction wall:1',
'Preload reaction wall:1','Preload reaction wall:1',#17312,#17329,
'Preload reaction wall:1');
#354=NEXT_ASSEMBLY_USAGE_OCCURRENCE('Front spring seat:1',
'Front spring seat:1','Front spring seat:1',#17312,#17330,
'Front spring seat:1');
#355=NEXT_ASSEMBLY_USAGE_OCCURRENCE('Rear spring shoe:1',
'Rear spring shoe:1','Rear spring shoe:1',#17312,#17331,
'Rear spring shoe:1');
#356=NEXT_ASSEMBLY_USAGE_OCCURRENCE('Preload spring:1',
'Preload spring:1','Preload spring:1',#17312,#17332,'Preload spring:1');
#357=NEXT_ASSEMBLY_USAGE_OCCURRENCE('Front spring seat (1):1',
'Front spring seat (1):1','Front spring seat (1):1',#17312,#17333,
'Front spring seat (1):1');
#358=NEXT_ASSEMBLY_USAGE_OCCURRENCE('Rear spring shoe (1):1',
'Rear spring shoe (1):1','Rear spring shoe (1):1',#17312,#17334,
'Rear spring shoe (1):1');
#359=NEXT_ASSEMBLY_USAGE_OCCURRENCE('Preload spring (1):1',
'Preload spring (1):1','Preload spring (1):1',#17312,#17335,
'Preload spring (1):1');
#360=NEXT_ASSEMBLY_USAGE_OCCURRENCE('Cap Screw - M5x20:2',
'Cap Screw - M5x20:2','Cap Screw - M5x20:2',#17312,#17336,
'Cap Screw - M5x20:2');
#361=NEXT_ASSEMBLY_USAGE_OCCURRENCE('Cap Screw - M5x20:3',
'Cap Screw - M5x20:3','Cap Screw - M5x20:3',#17312,#17336,
'Cap Screw - M5x20:3');
#362=NEXT_ASSEMBLY_USAGE_OCCURRENCE('Cap Screw - M5x20:4',
'Cap Screw - M5x20:4','Cap Screw - M5x20:4',#17312,#17336,
'Cap Screw - M5x20:4');
#363=NEXT_ASSEMBLY_USAGE_OCCURRENCE('Cap Screw - M5x20:5',
'Cap Screw - M5x20:5','Cap Screw - M5x20:5',#17312,#17336,
'Cap Screw - M5x20:5');
#364=NEXT_ASSEMBLY_USAGE_OCCURRENCE('Cap Screw - M4x16:2',
'Cap Screw - M4x16:2','Cap Screw - M4x16:2',#17312,#17353,
'Cap Screw - M4x16:2');
#365=NEXT_ASSEMBLY_USAGE_OCCURRENCE('Cap Screw - M4x16:3',
'Cap Screw - M4x16:3','Cap Screw - M4x16:3',#17312,#17353,
'Cap Screw - M4x16:3');
#366=NEXT_ASSEMBLY_USAGE_OCCURRENCE(
'Sealed Ball Bearing - 12 x 32 x 10 mm:2',
'Sealed Ball Bearing - 12 x 32 x 10 mm:2',
'Sealed Ball Bearing - 12 x 32 x 10 mm:2',#17312,#17337,
'Sealed Ball Bearing - 12 x 32 x 10 mm:2');
#367=NEXT_ASSEMBLY_USAGE_OCCURRENCE('M4x10 Cap Screw:2',
'M4x10 Cap Screw:2','M4x10 Cap Screw:2',#17312,#17343,
'M4x10 Cap Screw:2');
#368=NEXT_ASSEMBLY_USAGE_OCCURRENCE('M4x10 Cap Screw:3',
'M4x10 Cap Screw:3','M4x10 Cap Screw:3',#17312,#17343,
'M4x10 Cap Screw:3');
#369=NEXT_ASSEMBLY_USAGE_OCCURRENCE('M4x10 Cap Screw:4',
'M4x10 Cap Screw:4','M4x10 Cap Screw:4',#17312,#17343,
'M4x10 Cap Screw:4');
#370=NEXT_ASSEMBLY_USAGE_OCCURRENCE('M4x10 Cap Screw:5',
'M4x10 Cap Screw:5','M4x10 Cap Screw:5',#17312,#17343,
'M4x10 Cap Screw:5');
#371=NEXT_ASSEMBLY_USAGE_OCCURRENCE('M4x10 Cap Screw:6',
'M4x10 Cap Screw:6','M4x10 Cap Screw:6',#17312,#17343,
'M4x10 Cap Screw:6');
#372=NEXT_ASSEMBLY_USAGE_OCCURRENCE('M4x10 Cap Screw:7',
'M4x10 Cap Screw:7','M4x10 Cap Screw:7',#17312,#17343,
'M4x10 Cap Screw:7');
#373=NEXT_ASSEMBLY_USAGE_OCCURRENCE('M4x10 Cap Screw:8',
'M4x10 Cap Screw:8','M4x10 Cap Screw:8',#17312,#17343,
'M4x10 Cap Screw:8');
#374=NEXT_ASSEMBLY_USAGE_OCCURRENCE('M4x10 Cap Screw:9',
'M4x10 Cap Screw:9','M4x10 Cap Screw:9',#17312,#17343,
'M4x10 Cap Screw:9');
#375=NEXT_ASSEMBLY_USAGE_OCCURRENCE('Cap Screw - M4x16:4',
'Cap Screw - M4x16:4','Cap Screw - M4x16:4',#17312,#17353,
'Cap Screw - M4x16:4');
#376=NEXT_ASSEMBLY_USAGE_OCCURRENCE('Cap Screw - M4x16:5',
'Cap Screw - M4x16:5','Cap Screw - M4x16:5',#17312,#17353,
'Cap Screw - M4x16:5');
#377=NEXT_ASSEMBLY_USAGE_OCCURRENCE(
'Sealed Ball Bearing - 12 x 32 x 10 mm:3',
'Sealed Ball Bearing - 12 x 32 x 10 mm:3',
'Sealed Ball Bearing - 12 x 32 x 10 mm:3',#17312,#17337,
'Sealed Ball Bearing - 12 x 32 x 10 mm:3');
#378=NEXT_ASSEMBLY_USAGE_OCCURRENCE('M4x10 Cap Screw:10',
'M4x10 Cap Screw:10','M4x10 Cap Screw:10',#17312,#17343,
'M4x10 Cap Screw:10');
#379=NEXT_ASSEMBLY_USAGE_OCCURRENCE('M4x10 Cap Screw:11',
'M4x10 Cap Screw:11','M4x10 Cap Screw:11',#17312,#17343,
'M4x10 Cap Screw:11');
#380=NEXT_ASSEMBLY_USAGE_OCCURRENCE('M4x10 Cap Screw:12',
'M4x10 Cap Screw:12','M4x10 Cap Screw:12',#17312,#17343,
'M4x10 Cap Screw:12');
#381=NEXT_ASSEMBLY_USAGE_OCCURRENCE('M4x10 Cap Screw:13',
'M4x10 Cap Screw:13','M4x10 Cap Screw:13',#17312,#17343,
'M4x10 Cap Screw:13');
#382=NEXT_ASSEMBLY_USAGE_OCCURRENCE('M4x10 Cap Screw:14',
'M4x10 Cap Screw:14','M4x10 Cap Screw:14',#17312,#17343,
'M4x10 Cap Screw:14');
#383=NEXT_ASSEMBLY_USAGE_OCCURRENCE('M4x10 Cap Screw:15',
'M4x10 Cap Screw:15','M4x10 Cap Screw:15',#17312,#17343,
'M4x10 Cap Screw:15');
#384=NEXT_ASSEMBLY_USAGE_OCCURRENCE('M4x10 Cap Screw:16',
'M4x10 Cap Screw:16','M4x10 Cap Screw:16',#17312,#17343,
'M4x10 Cap Screw:16');
#385=NEXT_ASSEMBLY_USAGE_OCCURRENCE('M4x10 Cap Screw:17',
'M4x10 Cap Screw:17','M4x10 Cap Screw:17',#17312,#17343,
'M4x10 Cap Screw:17');
#386=NEXT_ASSEMBLY_USAGE_OCCURRENCE('Cap Screw - M4x16:6',
'Cap Screw - M4x16:6','Cap Screw - M4x16:6',#17312,#17353,
'Cap Screw - M4x16:6');
#387=NEXT_ASSEMBLY_USAGE_OCCURRENCE('Cap Screw - M4x16:7',
'Cap Screw - M4x16:7','Cap Screw - M4x16:7',#17312,#17353,
'Cap Screw - M4x16:7');
#388=NEXT_ASSEMBLY_USAGE_OCCURRENCE(
'Sealed Ball Bearing - 12 x 32 x 10 mm:4',
'Sealed Ball Bearing - 12 x 32 x 10 mm:4',
'Sealed Ball Bearing - 12 x 32 x 10 mm:4',#17312,#17337,
'Sealed Ball Bearing - 12 x 32 x 10 mm:4');
#389=NEXT_ASSEMBLY_USAGE_OCCURRENCE('M4x10 Cap Screw:18',
'M4x10 Cap Screw:18','M4x10 Cap Screw:18',#17312,#17343,
'M4x10 Cap Screw:18');
#390=NEXT_ASSEMBLY_USAGE_OCCURRENCE('M4x10 Cap Screw:19',
'M4x10 Cap Screw:19','M4x10 Cap Screw:19',#17312,#17343,
'M4x10 Cap Screw:19');
#391=NEXT_ASSEMBLY_USAGE_OCCURRENCE('M4x10 Cap Screw:20',
'M4x10 Cap Screw:20','M4x10 Cap Screw:20',#17312,#17343,
'M4x10 Cap Screw:20');
#392=NEXT_ASSEMBLY_USAGE_OCCURRENCE('M4x10 Cap Screw:21',
'M4x10 Cap Screw:21','M4x10 Cap Screw:21',#17312,#17343,
'M4x10 Cap Screw:21');
#393=NEXT_ASSEMBLY_USAGE_OCCURRENCE('M4x10 Cap Screw:22',
'M4x10 Cap Screw:22','M4x10 Cap Screw:22',#17312,#17343,
'M4x10 Cap Screw:22');
#394=NEXT_ASSEMBLY_USAGE_OCCURRENCE('M4x10 Cap Screw:23',
'M4x10 Cap Screw:23','M4x10 Cap Screw:23',#17312,#17343,
'M4x10 Cap Screw:23');
#395=NEXT_ASSEMBLY_USAGE_OCCURRENCE('M4x10 Cap Screw:24',
'M4x10 Cap Screw:24','M4x10 Cap Screw:24',#17312,#17343,
'M4x10 Cap Screw:24');
#396=NEXT_ASSEMBLY_USAGE_OCCURRENCE('M4x10 Cap Screw:25',
'M4x10 Cap Screw:25','M4x10 Cap Screw:25',#17312,#17343,
'M4x10 Cap Screw:25');
#397=NEXT_ASSEMBLY_USAGE_OCCURRENCE('Cap Screw - M4x16:8',
'Cap Screw - M4x16:8','Cap Screw - M4x16:8',#17312,#17353,
'Cap Screw - M4x16:8');
#398=NEXT_ASSEMBLY_USAGE_OCCURRENCE('Cap Screw - M4x16:9',
'Cap Screw - M4x16:9','Cap Screw - M4x16:9',#17312,#17353,
'Cap Screw - M4x16:9');
#399=NEXT_ASSEMBLY_USAGE_OCCURRENCE(
'Sealed Ball Bearing - 12 x 32 x 10 mm:5',
'Sealed Ball Bearing - 12 x 32 x 10 mm:5',
'Sealed Ball Bearing - 12 x 32 x 10 mm:5',#17312,#17337,
'Sealed Ball Bearing - 12 x 32 x 10 mm:5');
#400=NEXT_ASSEMBLY_USAGE_OCCURRENCE('M4x10 Cap Screw:26',
'M4x10 Cap Screw:26','M4x10 Cap Screw:26',#17312,#17343,
'M4x10 Cap Screw:26');
#401=NEXT_ASSEMBLY_USAGE_OCCURRENCE('M4x10 Cap Screw:27',
'M4x10 Cap Screw:27','M4x10 Cap Screw:27',#17312,#17343,
'M4x10 Cap Screw:27');
#402=NEXT_ASSEMBLY_USAGE_OCCURRENCE('M4x10 Cap Screw:28',
'M4x10 Cap Screw:28','M4x10 Cap Screw:28',#17312,#17343,
'M4x10 Cap Screw:28');
#403=NEXT_ASSEMBLY_USAGE_OCCURRENCE('M4x10 Cap Screw:29',
'M4x10 Cap Screw:29','M4x10 Cap Screw:29',#17312,#17343,
'M4x10 Cap Screw:29');
#404=NEXT_ASSEMBLY_USAGE_OCCURRENCE('M4x10 Cap Screw:30',
'M4x10 Cap Screw:30','M4x10 Cap Screw:30',#17312,#17343,
'M4x10 Cap Screw:30');
#405=NEXT_ASSEMBLY_USAGE_OCCURRENCE('M4x10 Cap Screw:31',
'M4x10 Cap Screw:31','M4x10 Cap Screw:31',#17312,#17343,
'M4x10 Cap Screw:31');
#406=NEXT_ASSEMBLY_USAGE_OCCURRENCE('M4x10 Cap Screw:32',
'M4x10 Cap Screw:32','M4x10 Cap Screw:32',#17312,#17343,
'M4x10 Cap Screw:32');
#407=NEXT_ASSEMBLY_USAGE_OCCURRENCE('M4x10 Cap Screw:33',
'M4x10 Cap Screw:33','M4x10 Cap Screw:33',#17312,#17343,
'M4x10 Cap Screw:33');
#408=NEXT_ASSEMBLY_USAGE_OCCURRENCE('Cap Screw - M4x16:11',
'Cap Screw - M4x16:11','Cap Screw - M4x16:11',#17312,#17353,
'Cap Screw - M4x16:11');
#409=NEXT_ASSEMBLY_USAGE_OCCURRENCE('Cap Screw - M4x16:12',
'Cap Screw - M4x16:12','Cap Screw - M4x16:12',#17312,#17353,
'Cap Screw - M4x16:12');
#410=NEXT_ASSEMBLY_USAGE_OCCURRENCE('Cap Screw - M6x25:2',
'Cap Screw - M6x25:2','Cap Screw - M6x25:2',#17312,#17344,
'Cap Screw - M6x25:2');
#411=NEXT_ASSEMBLY_USAGE_OCCURRENCE('Hex Nut - M6:2','Hex Nut - M6:2',
'Hex Nut - M6:2',#17312,#17345,'Hex Nut - M6:2');
#412=NEXT_ASSEMBLY_USAGE_OCCURRENCE('Cap Screw - M6x25:3',
'Cap Screw - M6x25:3','Cap Screw - M6x25:3',#17312,#17344,
'Cap Screw - M6x25:3');
#413=NEXT_ASSEMBLY_USAGE_OCCURRENCE('Hex Nut - M6:3','Hex Nut - M6:3',
'Hex Nut - M6:3',#17312,#17345,'Hex Nut - M6:3');
#414=NEXT_ASSEMBLY_USAGE_OCCURRENCE('Input shaft:1','Input shaft:1',
'Input shaft:1',#17346,#17347,'Input shaft:1');
#415=NEXT_ASSEMBLY_USAGE_OCCURRENCE('Input inner spacer:1',
'Input inner spacer:1','Input inner spacer:1',#17346,#17348,
'Input inner spacer:1');
#416=NEXT_ASSEMBLY_USAGE_OCCURRENCE('Input rear collar:1',
'Input rear collar:1','Input rear collar:1',#17346,#17349,
'Input rear collar:1');
#417=NEXT_ASSEMBLY_USAGE_OCCURRENCE('Face disc:1','Face disc:1',
'Face disc:1',#17346,#17350,'Face disc:1');
#418=NEXT_ASSEMBLY_USAGE_OCCURRENCE('Friction face:1','Friction face:1',
'Friction face:1',#17346,#17351,'Friction face:1');
#419=NEXT_ASSEMBLY_USAGE_OCCURRENCE('Input keeper:1','Input keeper:1',
'Input keeper:1',#17346,#17352,'Input keeper:1');
#420=NEXT_ASSEMBLY_USAGE_OCCURRENCE('M5x5 collar screw:2',
'M5x5 collar screw:2','M5x5 collar screw:2',#17346,#17362,
'M5x5 collar screw:2');
#421=NEXT_ASSEMBLY_USAGE_OCCURRENCE('Key 4x4x14:2','Key 4x4x14:2',
'Key 4x4x14:2',#17346,#17361,'Key 4x4x14:2');
#422=NEXT_ASSEMBLY_USAGE_OCCURRENCE('Cap Screw - M4x16:10',
'Cap Screw - M4x16:10','Cap Screw - M4x16:10',#17346,#17353,
'Cap Screw - M4x16:10');
#423=NEXT_ASSEMBLY_USAGE_OCCURRENCE('Output shaft:1','Output shaft:1',
'Output shaft:1',#17354,#17355,'Output shaft:1');
#424=NEXT_ASSEMBLY_USAGE_OCCURRENCE('Rim wheel:1','Rim wheel:1',
'Rim wheel:1',#17354,#17356,'Rim wheel:1');
#425=NEXT_ASSEMBLY_USAGE_OCCURRENCE('Friction rim band:1',
'Friction rim band:1','Friction rim band:1',#17354,#17357,
'Friction rim band:1');
#426=NEXT_ASSEMBLY_USAGE_OCCURRENCE('Output inner spacer:1',
'Output inner spacer:1','Output inner spacer:1',#17354,#17358,
'Output inner spacer:1');
#427=NEXT_ASSEMBLY_USAGE_OCCURRENCE('Output collar:1','Output collar:1',
'Output collar:1',#17354,#17359,'Output collar:1');
#428=NEXT_ASSEMBLY_USAGE_OCCURRENCE('Output collar (1):1',
'Output collar (1):1','Output collar (1):1',#17354,#17360,
'Output collar (1):1');
#429=NEXT_ASSEMBLY_USAGE_OCCURRENCE('Key 4x4x14:3','Key 4x4x14:3',
'Key 4x4x14:3',#17354,#17361,'Key 4x4x14:3');
#430=NEXT_ASSEMBLY_USAGE_OCCURRENCE('M5x5 collar screw:3',
'M5x5 collar screw:3','M5x5 collar screw:3',#17354,#17362,
'M5x5 collar screw:3');
#431=NEXT_ASSEMBLY_USAGE_OCCURRENCE('M5x5 collar screw:4',
'M5x5 collar screw:4','M5x5 collar screw:4',#17354,#17362,
'M5x5 collar screw:4');
#432=NEXT_ASSEMBLY_USAGE_OCCURRENCE('Frame and preload carriage:1',
'Frame and preload carriage:1','Frame and preload carriage:1',#17311,#17312,
'Frame and preload carriage:1');
#433=NEXT_ASSEMBLY_USAGE_OCCURRENCE('Face disc input:1',
'Face disc input:1','Face disc input:1',#17311,#17346,
'Face disc input:1');
#434=NEXT_ASSEMBLY_USAGE_OCCURRENCE('Rim wheel output:1',
'Rim wheel output:1','Rim wheel output:1',#17311,#17354,
'Rim wheel output:1');
#435=SPHERICAL_SURFACE('',#9303,0.29765);
#436=SPHERICAL_SURFACE('',#9305,0.29765);
#437=SPHERICAL_SURFACE('',#9307,0.29765);
#438=SPHERICAL_SURFACE('',#9309,0.29765);
#439=SPHERICAL_SURFACE('',#9311,0.29765);
#440=SPHERICAL_SURFACE('',#9313,0.29765);
#441=SPHERICAL_SURFACE('',#9315,0.29765);
#442=SPHERICAL_SURFACE('',#9318,0.309556);
#443=SPHERICAL_SURFACE('',#9334,0.309556);
#444=SPHERICAL_SURFACE('',#9339,0.309556);
#445=SPHERICAL_SURFACE('',#9345,0.309556);
#446=SPHERICAL_SURFACE('',#9350,0.309556);
#447=SPHERICAL_SURFACE('',#9355,0.309556);
#448=SPHERICAL_SURFACE('',#9363,0.309556);
#449=TOROIDAL_SURFACE('',#9263,1.1,0.309556);
#450=TOROIDAL_SURFACE('',#9283,1.1,0.309556);
#451=ORIENTED_CLOSED_SHELL('',*,#8190,.F.);
#452=ORIENTED_CLOSED_SHELL('',*,#8203,.F.);
#453=ORIENTED_CLOSED_SHELL('',*,#8206,.F.);
#454=ORIENTED_CLOSED_SHELL('',*,#8215,.F.);
#455=CONICAL_SURFACE('',#9238,0.4,0.785398163397448);
#456=CONICAL_SURFACE('',#9242,0.41,0.785398163397448);
#457=CONICAL_SURFACE('',#9246,0.26,0.463647609000806);
#458=CONICAL_SURFACE('',#9250,0.225,0.785398163397448);
#459=CONICAL_SURFACE('',#9274,0.63,0.785398163397448);
#460=CONICAL_SURFACE('',#9281,0.63,0.785398163397448);
#461=CONICAL_SURFACE('',#9294,1.57,0.785398163397449);
#462=CONICAL_SURFACE('',#9298,1.57,0.785398163397449);
#463=CONICAL_SURFACE('',#9402,0.325,0.785398163397448);
#464=CONICAL_SURFACE('',#9406,0.335,0.785398163397448);
#465=CONICAL_SURFACE('',#9410,0.21,0.463647609000806);
#466=CONICAL_SURFACE('',#9416,0.475,0.785398163397449);
#467=CONICAL_SURFACE('',#9420,0.485,0.785398163397448);
#468=CONICAL_SURFACE('',#9424,0.31,0.463647609000806);
#469=CONICAL_SURFACE('',#9428,0.27,0.785398163397448);
#470=CONICAL_SURFACE('',#9440,0.576175134594813,1.0471975511966);
#471=CONICAL_SURFACE('',#9442,0.576175134594813,1.0471975511966);
#472=CONICAL_SURFACE('',#9542,0.325,0.785398163397448);
#473=CONICAL_SURFACE('',#9546,0.335,0.785398163397448);
#474=CONICAL_SURFACE('',#9550,0.21,0.463647609000806);
#475=CONICAL_SURFACE('',#9554,0.18,0.785398163397448);
#476=CONICAL_SURFACE('',#9749,0.235,0.785398163397448);
#477=BREP_WITH_VOIDS('Body1',#8189,(#451));
#478=BREP_WITH_VOIDS('Body1',#8204,(#452));
#479=BREP_WITH_VOIDS('Body1',#8205,(#453));
#480=BREP_WITH_VOIDS('Body1',#8214,(#454));
#481=B_SPLINE_CURVE_WITH_KNOTS('',3,(#14322,#14323,#14324,#14325,#14326,
#14327,#14328,#14329,#14330,#14331,#14332,#14333,#14334,#14335,#14336,#14337,
#14338,#14339,#14340,#14341,#14342,#14343,#14344,#14345,#14346,#14347,#14348,
#14349,#14350,#14351,#14352,#14353,#14354,#14355,#14356,#14357,#14358,#14359,
#14360,#14361,#14362,#14363,#14364,#14365,#14366,#14367,#14368,#14369,#14370,
#14371,#14372,#14373,#14374,#14375,#14376,#14377,#14378,#14379,#14380,#14381,
#14382,#14383,#14384,#14385,#14386,#14387,#14388,#14389,#14390,#14391,#14392,
#14393,#14394,#14395,#14396,#14397,#14398,#14399,#14400,#14401,#14402,#14403,
#14404),.UNSPECIFIED.,.F.,.F.,(4,1,1,1,1,1,1,1,1,1,1,1,1,1,1,1,1,1,1,1,
1,1,1,1,1,1,1,1,1,1,1,1,1,1,1,1,1,1,1,1,1,1,1,1,1,1,1,1,1,1,1,1,1,1,1,1,
1,1,1,1,1,1,1,1,1,1,1,1,1,1,1,1,1,1,1,1,1,1,1,1,4),(0.,0.00892857142857143,
0.0178571428571429,0.0357142857142857,0.0535714285714286,0.0714285714285714,
0.0892857142857143,0.107142857142857,0.125,0.142857142857143,0.158730158730159,
0.174603174603175,0.19047619047619,0.202380952380952,0.214285714285714,
0.226190476190476,0.238095238095238,0.25,0.261904761904762,0.273809523809524,
0.285714285714286,0.297619047619048,0.30952380952381,0.321428571428571,
0.333333333333333,0.349206349206349,0.365079365079365,0.376984126984127,
0.380952380952381,0.392857142857143,0.404761904761905,0.416666666666667,
0.428571428571429,0.446428571428571,0.464285714285714,0.476190476190476,
0.488095238095238,0.5,0.508928571428571,0.517857142857143,0.526785714285714,
0.535714285714286,0.553571428571429,0.571428571428571,0.589285714285714,
0.607142857142857,0.625,0.633928571428571,0.642857142857143,0.654761904761905,
0.666666666666667,0.678571428571428,0.6875,0.696428571428571,0.705357142857143,
0.714285714285714,0.726190476190476,0.738095238095238,0.75,0.761904761904762,
0.773809523809524,0.785714285714286,0.791666666666667,0.797619047619047,
0.803571428571428,0.809523809523809,0.821428571428571,0.833333333333333,
0.845238095238095,0.857142857142857,0.866071428571429,0.875,0.883928571428571,
0.892857142857143,0.910714285714286,0.928571428571429,0.946428571428571,
0.964285714285714,0.982142857142857,0.991071428571429,1.),.UNSPECIFIED.);
#482=B_SPLINE_CURVE_WITH_KNOTS('',3,(#15240,#15241,#15242,#15243,#15244,
#15245,#15246,#15247,#15248,#15249,#15250,#15251,#15252,#15253,#15254,#15255,
#15256,#15257,#15258,#15259,#15260,#15261,#15262,#15263,#15264,#15265,#15266,
#15267,#15268,#15269,#15270,#15271,#15272,#15273,#15274,#15275,#15276,#15277,
#15278,#15279,#15280,#15281,#15282,#15283,#15284,#15285,#15286,#15287,#15288,
#15289,#15290,#15291,#15292,#15293,#15294,#15295,#15296,#15297,#15298,#15299,
#15300,#15301,#15302,#15303,#15304,#15305,#15306,#15307,#15308,#15309,#15310,
#15311,#15312,#15313,#15314,#15315,#15316,#15317,#15318,#15319,#15320),
 .UNSPECIFIED.,.F.,.F.,(4,1,1,1,1,1,1,1,1,1,1,1,1,1,1,1,1,1,1,1,1,1,1,1,
1,1,1,1,1,1,1,1,1,1,1,1,1,1,1,1,1,1,1,1,1,1,1,1,1,1,1,1,1,1,1,1,1,1,1,1,
1,1,1,1,1,1,1,1,1,1,1,1,1,1,1,1,1,1,4),(0.,0.00892857142857143,0.0178571428571429,
0.0357142857142857,0.0535714285714286,0.0714285714285714,0.0892857142857143,
0.107142857142857,0.125,0.142857142857143,0.158730158730159,0.174603174603175,
0.19047619047619,0.202380952380952,0.214285714285714,0.220238095238095,
0.226190476190476,0.238095238095238,0.25,0.261904761904762,0.273809523809524,
0.285714285714286,0.297619047619048,0.30952380952381,0.321428571428571,
0.333333333333333,0.349206349206349,0.365079365079365,0.376984126984127,
0.380952380952381,0.392857142857143,0.404761904761905,0.416666666666667,
0.428571428571429,0.446428571428571,0.464285714285714,0.476190476190476,
0.485119047619048,0.5,0.508928571428571,0.517857142857143,0.535714285714286,
0.553571428571429,0.571428571428571,0.589285714285714,0.607142857142857,
0.625,0.642857142857143,0.651785714285714,0.654761904761905,0.666666666666667,
0.678571428571428,0.696428571428571,0.705357142857143,0.714285714285714,
0.726190476190476,0.738095238095238,0.75,0.761904761904762,0.773809523809524,
0.785714285714286,0.797619047619047,0.803571428571428,0.806547619047619,
0.809523809523809,0.821428571428571,0.833333333333333,0.845238095238095,
0.857142857142857,0.866071428571429,0.875,0.892857142857143,0.910714285714286,
0.928571428571429,0.946428571428571,0.964285714285714,0.982142857142857,
0.991071428571429,1.),.UNSPECIFIED.);
#483=B_SPLINE_CURVE_WITH_KNOTS('',3,(#15498,#15499,#15500,#15501,#15502,
#15503,#15504,#15505,#15506,#15507,#15508,#15509,#15510,#15511,#15512,#15513,
#15514,#15515,#15516,#15517,#15518,#15519),.UNSPECIFIED.,.F.,.F.,(4,2,2,
2,2,2,2,2,2,2,4),(0.0591825211272536,0.157966726598481,0.236950089897721,
0.315933453196962,0.391576304923761,0.46721915665056,0.54286200837736,0.618504860104159,
0.697488223403399,0.77647158670264,0.875255792173867),.UNSPECIFIED.);
#484=B_SPLINE_CURVE_WITH_KNOTS('',3,(#15523,#15524,#15525,#15526,#15527,
#15528,#15529,#15530,#15531,#15532,#15533,#15534,#15535,#15536,#15537,#15538,
#15539,#15540,#15541,#15542,#15543,#15544),.UNSPECIFIED.,.F.,.F.,(4,2,2,
2,2,2,2,2,2,2,4),(0.0581119756758434,0.106553146291161,0.213106292582322,
0.30849933801665,0.386091982889075,0.4636846277615,0.541277272633925,0.61886991750635,
0.714262962940678,0.820816109231839,0.869257279847157),.UNSPECIFIED.);
#485=B_SPLINE_CURVE_WITH_KNOTS('',3,(#15550,#15551,#15552,#15553,#15554,
#15555,#15556,#15557,#15558,#15559,#15560,#15561,#15562,#15563,#15564,#15565,
#15566,#15567,#15568,#15569,#15570,#15571),.UNSPECIFIED.,.F.,.F.,(4,2,2,
2,2,2,2,2,2,2,4),(0.0581119756758434,0.106553146291161,0.213106292582322,
0.30849933801665,0.386091982889075,0.4636846277615,0.541277272633925,0.61886991750635,
0.714262962940679,0.820816109231839,0.869257279847157),.UNSPECIFIED.);
#486=B_SPLINE_CURVE_WITH_KNOTS('',3,(#15575,#15576,#15577,#15578,#15579,
#15580,#15581,#15582,#15583,#15584,#15585,#15586,#15587,#15588,#15589,#15590,
#15591,#15592,#15593,#15594,#15595,#15596),.UNSPECIFIED.,.F.,.F.,(4,2,2,
2,2,2,2,2,2,2,4),(0.0581119756758433,0.106553146291161,0.213106292582322,
0.308499338016649,0.386091982889075,0.4636846277615,0.541277272633925,0.61886991750635,
0.714262962940678,0.820816109231839,0.869257279847157),.UNSPECIFIED.);
#487=B_SPLINE_CURVE_WITH_KNOTS('',3,(#15605,#15606,#15607,#15608,#15609,
#15610,#15611,#15612,#15613,#15614,#15615,#15616,#15617,#15618,#15619,#15620,
#15621,#15622,#15623,#15624,#15625,#15626),.UNSPECIFIED.,.F.,.F.,(4,2,2,
2,2,2,2,2,2,2,4),(0.0581119756758433,0.106553146291161,0.213106292582322,
0.30849933801665,0.386091982889075,0.4636846277615,0.541277272633925,0.61886991750635,
0.714262962940678,0.820816109231839,0.869257279847157),.UNSPECIFIED.);
#488=B_SPLINE_CURVE_WITH_KNOTS('',3,(#15630,#15631,#15632,#15633,#15634,
#15635,#15636,#15637,#15638,#15639,#15640,#15641,#15642,#15643,#15644,#15645,
#15646,#15647,#15648,#15649,#15650,#15651),.UNSPECIFIED.,.F.,.F.,(4,2,2,
2,2,2,2,2,2,2,4),(0.0581119756758434,0.106553146291161,0.213106292582322,
0.30849933801665,0.386091982889075,0.4636846277615,0.541277272633925,0.61886991750635,
0.714262962940678,0.820816109231839,0.869257279847157),.UNSPECIFIED.);
#489=B_SPLINE_CURVE_WITH_KNOTS('',3,(#15655,#15656,#15657,#15658,#15659,
#15660,#15661,#15662,#15663,#15664,#15665,#15666,#15667,#15668,#15669,#15670,
#15671,#15672,#15673,#15674,#15675,#15676),.UNSPECIFIED.,.F.,.F.,(4,2,2,
2,2,2,2,2,2,2,4),(0.0581119756758434,0.106553146291161,0.213106292582322,
0.30849933801665,0.386091982889075,0.4636846277615,0.541277272633925,0.61886991750635,
0.714262962940678,0.820816109231839,0.869257279847157),.UNSPECIFIED.);
#490=B_SPLINE_CURVE_WITH_KNOTS('',3,(#15680,#15681,#15682,#15683,#15684,
#15685,#15686,#15687,#15688,#15689,#15690,#15691,#15692,#15693,#15694,#15695,
#15696,#15697,#15698,#15699,#15700,#15701),.UNSPECIFIED.,.F.,.F.,(4,2,2,
2,2,2,2,2,2,2,4),(0.0581119756758433,0.106553146291161,0.213106292582322,
0.30849933801665,0.386091982889075,0.4636846277615,0.541277272633925,0.61886991750635,
0.714262962940678,0.820816109231839,0.869257279847157),.UNSPECIFIED.);
#491=B_SPLINE_CURVE_WITH_KNOTS('',3,(#15709,#15710,#15711,#15712,#15713,
#15714,#15715,#15716,#15717,#15718,#15719,#15720,#15721,#15722,#15723,#15724,
#15725,#15726,#15727,#15728,#15729,#15730),.UNSPECIFIED.,.F.,.F.,(4,2,2,
2,2,2,2,2,2,2,4),(0.0591825211272536,0.157966726598481,0.236950089897721,
0.315933453196962,0.391576304923761,0.467219156650561,0.54286200837736,
0.618504860104159,0.697488223403399,0.77647158670264,0.875255792173867),
 .UNSPECIFIED.);
#492=B_SPLINE_CURVE_WITH_KNOTS('',3,(#15738,#15739,#15740,#15741,#15742,
#15743,#15744,#15745,#15746,#15747,#15748,#15749,#15750,#15751,#15752,#15753,
#15754,#15755,#15756,#15757,#15758,#15759),.UNSPECIFIED.,.F.,.F.,(4,2,2,
2,2,2,2,2,2,2,4),(0.0591825211272536,0.157966726598481,0.236950089897722,
0.315933453196962,0.391576304923761,0.467219156650561,0.54286200837736,
0.618504860104159,0.697488223403399,0.77647158670264,0.875255792173867),
 .UNSPECIFIED.);
#493=B_SPLINE_CURVE_WITH_KNOTS('',3,(#15769,#15770,#15771,#15772,#15773,
#15774,#15775,#15776,#15777,#15778,#15779,#15780,#15781,#15782,#15783,#15784,
#15785,#15786,#15787,#15788,#15789,#15790),.UNSPECIFIED.,.F.,.F.,(4,2,2,
2,2,2,2,2,2,2,4),(0.0591825211272536,0.157966726598481,0.236950089897721,
0.315933453196962,0.391576304923761,0.46721915665056,0.54286200837736,0.618504860104159,
0.697488223403399,0.77647158670264,0.875255792173867),.UNSPECIFIED.);
#494=B_SPLINE_CURVE_WITH_KNOTS('',3,(#15798,#15799,#15800,#15801,#15802,
#15803,#15804,#15805,#15806,#15807,#15808,#15809,#15810,#15811,#15812,#15813,
#15814,#15815,#15816,#15817,#15818,#15819),.UNSPECIFIED.,.F.,.F.,(4,2,2,
2,2,2,2,2,2,2,4),(0.0591825211272536,0.157966726598481,0.236950089897721,
0.315933453196962,0.391576304923761,0.46721915665056,0.542862008377359,
0.618504860104159,0.697488223403399,0.776471586702639,0.875255792173867),
 .UNSPECIFIED.);
#495=B_SPLINE_CURVE_WITH_KNOTS('',3,(#15827,#15828,#15829,#15830,#15831,
#15832,#15833,#15834,#15835,#15836,#15837,#15838,#15839,#15840,#15841,#15842,
#15843,#15844,#15845,#15846,#15847,#15848),.UNSPECIFIED.,.F.,.F.,(4,2,2,
2,2,2,2,2,2,2,4),(0.0591825211272536,0.157966726598481,0.236950089897721,
0.315933453196962,0.391576304923761,0.46721915665056,0.54286200837736,0.618504860104159,
0.697488223403399,0.77647158670264,0.875255792173867),.UNSPECIFIED.);
#496=B_SPLINE_CURVE_WITH_KNOTS('',3,(#15857,#15858,#15859,#15860,#15861,
#15862,#15863,#15864,#15865,#15866,#15867,#15868,#15869,#15870,#15871,#15872,
#15873,#15874,#15875,#15876,#15877,#15878),.UNSPECIFIED.,.F.,.F.,(4,2,2,
2,2,2,2,2,2,2,4),(0.0591825211272536,0.157966726598481,0.236950089897721,
0.315933453196962,0.391576304923761,0.46721915665056,0.542862008377359,
0.618504860104159,0.697488223403399,0.776471586702639,0.875255792173867),
 .UNSPECIFIED.);
#497=B_SPLINE_CURVE_WITH_KNOTS('',3,(#16212,#16213,#16214,#16215,#16216,
#16217,#16218,#16219,#16220,#16221),.UNSPECIFIED.,.F.,.F.,(4,2,2,2,4),(0.818088904349172,
0.878131747417165,0.957937926194036,1.03774410497091,1.0977869480389),
 .UNSPECIFIED.);
#498=B_SPLINE_CURVE_WITH_KNOTS('',3,(#16227,#16228,#16229,#16230,#16231,
#16232,#16233,#16234,#16235,#16236,#16237,#16238,#16239,#16240,#16241,#16242,
#16243,#16244),.UNSPECIFIED.,.F.,.F.,(4,2,2,2,2,2,2,2,4),(0.,0.0793157643915219,
0.158631528783044,0.23794361593365,0.317255703084256,0.396567790234861,
0.475879877385467,0.555195641776989,0.634511406168511),.UNSPECIFIED.);
#499=B_SPLINE_CURVE_WITH_KNOTS('',3,(#16245,#16246,#16247,#16248,#16249,
#16250,#16251,#16252,#16253,#16254,#16255,#16256,#16257,#16258,#16259,#16260,
#16261,#16262),.UNSPECIFIED.,.F.,.F.,(4,2,2,2,2,2,2,2,4),(0.634511406168511,
0.713827170560033,0.793142934951555,0.872455022102161,0.951767109252766,
1.03107919640337,1.11039128355398,1.1897070479455,1.26902281233702),
 .UNSPECIFIED.);
#500=B_SPLINE_CURVE_WITH_KNOTS('',3,(#16265,#16266,#16267,#16268,#16269,
#16270,#16271,#16272,#16273,#16274),.UNSPECIFIED.,.F.,.F.,(4,2,2,2,4),(0.179463620219816,
0.239506463287808,0.319312642064679,0.399118820841549,0.459161663909541),
 .UNSPECIFIED.);
#501=B_SPLINE_CURVE_WITH_KNOTS('',3,(#16636,#16637,#16638,#16639,#16640,
#16641),.UNSPECIFIED.,.F.,.F.,(4,2,4),(0.818088904349169,0.878131747417164,
0.957937926194035),.UNSPECIFIED.);
#502=B_SPLINE_CURVE_WITH_KNOTS('',3,(#16645,#16646,#16647,#16648,#16649,
#16650),.UNSPECIFIED.,.F.,.F.,(4,2,4),(0.319312642064678,0.399118820841549,
0.459161663909543),.UNSPECIFIED.);
#503=B_SPLINE_CURVE_WITH_KNOTS('',3,(#16651,#16652,#16653,#16654,#16655,
#16656),.UNSPECIFIED.,.F.,.F.,(4,2,4),(0.179463620219813,0.239506463287807,
0.319312642064678),.UNSPECIFIED.);
#504=B_SPLINE_CURVE_WITH_KNOTS('',3,(#16657,#16658,#16659,#16660,#16661,
#16662),.UNSPECIFIED.,.F.,.F.,(4,2,4),(0.957937926194035,1.03774410497091,
1.0977869480389),.UNSPECIFIED.);
#505=B_SPLINE_CURVE_WITH_KNOTS('',3,(#16666,#16667,#16668,#16669,#16670,
#16671,#16672,#16673,#16674,#16675),.UNSPECIFIED.,.F.,.F.,(4,2,2,2,4),(0.,
0.0793157643915217,0.158631528783043,0.237943615933649,0.317255703084255),
 .UNSPECIFIED.);
#506=B_SPLINE_CURVE_WITH_KNOTS('',3,(#16677,#16678,#16679,#16680,#16681,
#16682,#16683,#16684,#16685,#16686),.UNSPECIFIED.,.F.,.F.,(4,2,2,2,4),(0.951767109252766,
1.03107919640337,1.11039128355398,1.1897070479455,1.26902281233702),
 .UNSPECIFIED.);
#507=B_SPLINE_CURVE_WITH_KNOTS('',3,(#16687,#16688,#16689,#16690,#16691,
#16692,#16693,#16694,#16695,#16696,#16697,#16698,#16699,#16700,#16701,#16702,
#16703,#16704),.UNSPECIFIED.,.F.,.F.,(4,2,2,2,2,2,2,2,4),(0.317255703084255,
0.396567790234861,0.475879877385467,0.555195641776989,0.63451140616851,
0.713827170560032,0.793142934951554,0.87245502210216,0.951767109252766),
 .UNSPECIFIED.);
#508=B_SPLINE_CURVE_WITH_KNOTS('',3,(#16732,#16733,#16734,#16735,#16736,
#16737),.UNSPECIFIED.,.F.,.F.,(4,2,4),(0.818088904349171,0.878131747417164,
0.957937926194035),.UNSPECIFIED.);
#509=B_SPLINE_CURVE_WITH_KNOTS('',3,(#16741,#16742,#16743,#16744,#16745,
#16746),.UNSPECIFIED.,.F.,.F.,(4,2,4),(0.319312642064678,0.399118820841549,
0.459161663909542),.UNSPECIFIED.);
#510=B_SPLINE_CURVE_WITH_KNOTS('',3,(#16747,#16748,#16749,#16750,#16751,
#16752),.UNSPECIFIED.,.F.,.F.,(4,2,4),(0.179463620219812,0.239506463287808,
0.319312642064678),.UNSPECIFIED.);
#511=B_SPLINE_CURVE_WITH_KNOTS('',3,(#16753,#16754,#16755,#16756,#16757,
#16758),.UNSPECIFIED.,.F.,.F.,(4,2,4),(0.957937926194035,1.03774410497091,
1.0977869480389),.UNSPECIFIED.);
#512=B_SPLINE_CURVE_WITH_KNOTS('',3,(#16762,#16763,#16764,#16765,#16766,
#16767,#16768,#16769,#16770,#16771),.UNSPECIFIED.,.F.,.F.,(4,2,2,2,4),(0.,
0.0793157643915219,0.158631528783044,0.23794361593365,0.317255703084255),
 .UNSPECIFIED.);
#513=B_SPLINE_CURVE_WITH_KNOTS('',3,(#16773,#16774,#16775,#16776,#16777,
#16778,#16779,#16780,#16781,#16782),.UNSPECIFIED.,.F.,.F.,(4,2,2,2,4),(0.951767109252766,
1.03107919640337,1.11039128355398,1.1897070479455,1.26902281233702),
 .UNSPECIFIED.);
#514=B_SPLINE_CURVE_WITH_KNOTS('',3,(#16783,#16784,#16785,#16786,#16787,
#16788,#16789,#16790,#16791,#16792,#16793,#16794,#16795,#16796,#16797,#16798,
#16799,#16800),.UNSPECIFIED.,.F.,.F.,(4,2,2,2,2,2,2,2,4),(0.317255703084255,
0.396567790234861,0.475879877385467,0.555195641776989,0.634511406168511,
0.713827170560032,0.793142934951554,0.87245502210216,0.951767109252766),
 .UNSPECIFIED.);
#515=B_SPLINE_SURFACE_WITH_KNOTS('',3,3,((#13489,#13490,#13491,#13492,#13493,
#13494,#13495,#13496,#13497,#13498,#13499,#13500,#13501,#13502,#13503,#13504,
#13505,#13506,#13507,#13508,#13509,#13510,#13511,#13512,#13513,#13514,#13515,
#13516,#13517,#13518,#13519,#13520,#13521,#13522,#13523,#13524,#13525,#13526,
#13527,#13528,#13529,#13530,#13531,#13532,#13533,#13534,#13535,#13536,#13537,
#13538,#13539,#13540,#13541,#13542,#13543,#13544,#13545,#13546,#13547,#13548,
#13549,#13550,#13551,#13552,#13553,#13554,#13555,#13556,#13557,#13558,#13559,
#13560,#13561,#13562,#13563,#13564,#13565,#13566,#13567,#13568,#13569,#13570,
#13571),(#13572,#13573,#13574,#13575,#13576,#13577,#13578,#13579,#13580,
#13581,#13582,#13583,#13584,#13585,#13586,#13587,#13588,#13589,#13590,#13591,
#13592,#13593,#13594,#13595,#13596,#13597,#13598,#13599,#13600,#13601,#13602,
#13603,#13604,#13605,#13606,#13607,#13608,#13609,#13610,#13611,#13612,#13613,
#13614,#13615,#13616,#13617,#13618,#13619,#13620,#13621,#13622,#13623,#13624,
#13625,#13626,#13627,#13628,#13629,#13630,#13631,#13632,#13633,#13634,#13635,
#13636,#13637,#13638,#13639,#13640,#13641,#13642,#13643,#13644,#13645,#13646,
#13647,#13648,#13649,#13650,#13651,#13652,#13653,#13654),(#13655,#13656,
#13657,#13658,#13659,#13660,#13661,#13662,#13663,#13664,#13665,#13666,#13667,
#13668,#13669,#13670,#13671,#13672,#13673,#13674,#13675,#13676,#13677,#13678,
#13679,#13680,#13681,#13682,#13683,#13684,#13685,#13686,#13687,#13688,#13689,
#13690,#13691,#13692,#13693,#13694,#13695,#13696,#13697,#13698,#13699,#13700,
#13701,#13702,#13703,#13704,#13705,#13706,#13707,#13708,#13709,#13710,#13711,
#13712,#13713,#13714,#13715,#13716,#13717,#13718,#13719,#13720,#13721,#13722,
#13723,#13724,#13725,#13726,#13727,#13728,#13729,#13730,#13731,#13732,#13733,
#13734,#13735,#13736,#13737),(#13738,#13739,#13740,#13741,#13742,#13743,
#13744,#13745,#13746,#13747,#13748,#13749,#13750,#13751,#13752,#13753,#13754,
#13755,#13756,#13757,#13758,#13759,#13760,#13761,#13762,#13763,#13764,#13765,
#13766,#13767,#13768,#13769,#13770,#13771,#13772,#13773,#13774,#13775,#13776,
#13777,#13778,#13779,#13780,#13781,#13782,#13783,#13784,#13785,#13786,#13787,
#13788,#13789,#13790,#13791,#13792,#13793,#13794,#13795,#13796,#13797,#13798,
#13799,#13800,#13801,#13802,#13803,#13804,#13805,#13806,#13807,#13808,#13809,
#13810,#13811,#13812,#13813,#13814,#13815,#13816,#13817,#13818,#13819,#13820),
(#13821,#13822,#13823,#13824,#13825,#13826,#13827,#13828,#13829,#13830,
#13831,#13832,#13833,#13834,#13835,#13836,#13837,#13838,#13839,#13840,#13841,
#13842,#13843,#13844,#13845,#13846,#13847,#13848,#13849,#13850,#13851,#13852,
#13853,#13854,#13855,#13856,#13857,#13858,#13859,#13860,#13861,#13862,#13863,
#13864,#13865,#13866,#13867,#13868,#13869,#13870,#13871,#13872,#13873,#13874,
#13875,#13876,#13877,#13878,#13879,#13880,#13881,#13882,#13883,#13884,#13885,
#13886,#13887,#13888,#13889,#13890,#13891,#13892,#13893,#13894,#13895,#13896,
#13897,#13898,#13899,#13900,#13901,#13902,#13903),(#13904,#13905,#13906,
#13907,#13908,#13909,#13910,#13911,#13912,#13913,#13914,#13915,#13916,#13917,
#13918,#13919,#13920,#13921,#13922,#13923,#13924,#13925,#13926,#13927,#13928,
#13929,#13930,#13931,#13932,#13933,#13934,#13935,#13936,#13937,#13938,#13939,
#13940,#13941,#13942,#13943,#13944,#13945,#13946,#13947,#13948,#13949,#13950,
#13951,#13952,#13953,#13954,#13955,#13956,#13957,#13958,#13959,#13960,#13961,
#13962,#13963,#13964,#13965,#13966,#13967,#13968,#13969,#13970,#13971,#13972,
#13973,#13974,#13975,#13976,#13977,#13978,#13979,#13980,#13981,#13982,#13983,
#13984,#13985,#13986),(#13987,#13988,#13989,#13990,#13991,#13992,#13993,
#13994,#13995,#13996,#13997,#13998,#13999,#14000,#14001,#14002,#14003,#14004,
#14005,#14006,#14007,#14008,#14009,#14010,#14011,#14012,#14013,#14014,#14015,
#14016,#14017,#14018,#14019,#14020,#14021,#14022,#14023,#14024,#14025,#14026,
#14027,#14028,#14029,#14030,#14031,#14032,#14033,#14034,#14035,#14036,#14037,
#14038,#14039,#14040,#14041,#14042,#14043,#14044,#14045,#14046,#14047,#14048,
#14049,#14050,#14051,#14052,#14053,#14054,#14055,#14056,#14057,#14058,#14059,
#14060,#14061,#14062,#14063,#14064,#14065,#14066,#14067,#14068,#14069),
(#14070,#14071,#14072,#14073,#14074,#14075,#14076,#14077,#14078,#14079,
#14080,#14081,#14082,#14083,#14084,#14085,#14086,#14087,#14088,#14089,#14090,
#14091,#14092,#14093,#14094,#14095,#14096,#14097,#14098,#14099,#14100,#14101,
#14102,#14103,#14104,#14105,#14106,#14107,#14108,#14109,#14110,#14111,#14112,
#14113,#14114,#14115,#14116,#14117,#14118,#14119,#14120,#14121,#14122,#14123,
#14124,#14125,#14126,#14127,#14128,#14129,#14130,#14131,#14132,#14133,#14134,
#14135,#14136,#14137,#14138,#14139,#14140,#14141,#14142,#14143,#14144,#14145,
#14146,#14147,#14148,#14149,#14150,#14151,#14152),(#14153,#14154,#14155,
#14156,#14157,#14158,#14159,#14160,#14161,#14162,#14163,#14164,#14165,#14166,
#14167,#14168,#14169,#14170,#14171,#14172,#14173,#14174,#14175,#14176,#14177,
#14178,#14179,#14180,#14181,#14182,#14183,#14184,#14185,#14186,#14187,#14188,
#14189,#14190,#14191,#14192,#14193,#14194,#14195,#14196,#14197,#14198,#14199,
#14200,#14201,#14202,#14203,#14204,#14205,#14206,#14207,#14208,#14209,#14210,
#14211,#14212,#14213,#14214,#14215,#14216,#14217,#14218,#14219,#14220,#14221,
#14222,#14223,#14224,#14225,#14226,#14227,#14228,#14229,#14230,#14231,#14232,
#14233,#14234,#14235),(#14236,#14237,#14238,#14239,#14240,#14241,#14242,
#14243,#14244,#14245,#14246,#14247,#14248,#14249,#14250,#14251,#14252,#14253,
#14254,#14255,#14256,#14257,#14258,#14259,#14260,#14261,#14262,#14263,#14264,
#14265,#14266,#14267,#14268,#14269,#14270,#14271,#14272,#14273,#14274,#14275,
#14276,#14277,#14278,#14279,#14280,#14281,#14282,#14283,#14284,#14285,#14286,
#14287,#14288,#14289,#14290,#14291,#14292,#14293,#14294,#14295,#14296,#14297,
#14298,#14299,#14300,#14301,#14302,#14303,#14304,#14305,#14306,#14307,#14308,
#14309,#14310,#14311,#14312,#14313,#14314,#14315,#14316,#14317,#14318)),
 .UNSPECIFIED.,.T.,.F.,.F.,(4,1,1,1,1,1,1,4),(4,1,1,1,1,1,1,1,1,1,1,1,1,
1,1,1,1,1,1,1,1,1,1,1,1,1,1,1,1,1,1,1,1,1,1,1,1,1,1,1,1,1,1,1,1,1,1,1,1,
1,1,1,1,1,1,1,1,1,1,1,1,1,1,1,1,1,1,1,1,1,1,1,1,1,1,1,1,1,1,1,4),(-3.14159265358979,
-2.24399475256414,-1.34639685153848,-0.448798950512828,0.448798950512828,
1.34639685153848,2.24399475256414,3.14159265358979),(0.,0.00892857142857143,
0.0178571428571429,0.0357142857142857,0.0535714285714286,0.0714285714285714,
0.0892857142857143,0.107142857142857,0.125,0.142857142857143,0.158730158730159,
0.174603174603175,0.19047619047619,0.202380952380952,0.214285714285714,
0.226190476190476,0.238095238095238,0.25,0.261904761904762,0.273809523809524,
0.285714285714286,0.297619047619048,0.30952380952381,0.321428571428571,
0.333333333333333,0.349206349206349,0.365079365079365,0.376984126984127,
0.380952380952381,0.392857142857143,0.404761904761905,0.416666666666667,
0.428571428571429,0.446428571428571,0.464285714285714,0.476190476190476,
0.488095238095238,0.5,0.508928571428571,0.517857142857143,0.526785714285714,
0.535714285714286,0.553571428571429,0.571428571428571,0.589285714285714,
0.607142857142857,0.625,0.633928571428571,0.642857142857143,0.654761904761905,
0.666666666666667,0.678571428571428,0.6875,0.696428571428571,0.705357142857143,
0.714285714285714,0.726190476190476,0.738095238095238,0.75,0.761904761904762,
0.773809523809524,0.785714285714286,0.791666666666667,0.797619047619047,
0.803571428571428,0.809523809523809,0.821428571428571,0.833333333333333,
0.845238095238095,0.857142857142857,0.866071428571429,0.875,0.883928571428571,
0.892857142857143,0.910714285714286,0.928571428571429,0.946428571428571,
0.964285714285714,0.982142857142857,0.991071428571429,1.),.UNSPECIFIED.);
#516=B_SPLINE_SURFACE_WITH_KNOTS('',3,3,((#14427,#14428,#14429,#14430,#14431,
#14432,#14433,#14434,#14435,#14436,#14437,#14438,#14439,#14440,#14441,#14442,
#14443,#14444,#14445,#14446,#14447,#14448,#14449,#14450,#14451,#14452,#14453,
#14454,#14455,#14456,#14457,#14458,#14459,#14460,#14461,#14462,#14463,#14464,
#14465,#14466,#14467,#14468,#14469,#14470,#14471,#14472,#14473,#14474,#14475,
#14476,#14477,#14478,#14479,#14480,#14481,#14482,#14483,#14484,#14485,#14486,
#14487,#14488,#14489,#14490,#14491,#14492,#14493,#14494,#14495,#14496,#14497,
#14498,#14499,#14500,#14501,#14502,#14503,#14504,#14505,#14506,#14507),
(#14508,#14509,#14510,#14511,#14512,#14513,#14514,#14515,#14516,#14517,
#14518,#14519,#14520,#14521,#14522,#14523,#14524,#14525,#14526,#14527,#14528,
#14529,#14530,#14531,#14532,#14533,#14534,#14535,#14536,#14537,#14538,#14539,
#14540,#14541,#14542,#14543,#14544,#14545,#14546,#14547,#14548,#14549,#14550,
#14551,#14552,#14553,#14554,#14555,#14556,#14557,#14558,#14559,#14560,#14561,
#14562,#14563,#14564,#14565,#14566,#14567,#14568,#14569,#14570,#14571,#14572,
#14573,#14574,#14575,#14576,#14577,#14578,#14579,#14580,#14581,#14582,#14583,
#14584,#14585,#14586,#14587,#14588),(#14589,#14590,#14591,#14592,#14593,
#14594,#14595,#14596,#14597,#14598,#14599,#14600,#14601,#14602,#14603,#14604,
#14605,#14606,#14607,#14608,#14609,#14610,#14611,#14612,#14613,#14614,#14615,
#14616,#14617,#14618,#14619,#14620,#14621,#14622,#14623,#14624,#14625,#14626,
#14627,#14628,#14629,#14630,#14631,#14632,#14633,#14634,#14635,#14636,#14637,
#14638,#14639,#14640,#14641,#14642,#14643,#14644,#14645,#14646,#14647,#14648,
#14649,#14650,#14651,#14652,#14653,#14654,#14655,#14656,#14657,#14658,#14659,
#14660,#14661,#14662,#14663,#14664,#14665,#14666,#14667,#14668,#14669),
(#14670,#14671,#14672,#14673,#14674,#14675,#14676,#14677,#14678,#14679,
#14680,#14681,#14682,#14683,#14684,#14685,#14686,#14687,#14688,#14689,#14690,
#14691,#14692,#14693,#14694,#14695,#14696,#14697,#14698,#14699,#14700,#14701,
#14702,#14703,#14704,#14705,#14706,#14707,#14708,#14709,#14710,#14711,#14712,
#14713,#14714,#14715,#14716,#14717,#14718,#14719,#14720,#14721,#14722,#14723,
#14724,#14725,#14726,#14727,#14728,#14729,#14730,#14731,#14732,#14733,#14734,
#14735,#14736,#14737,#14738,#14739,#14740,#14741,#14742,#14743,#14744,#14745,
#14746,#14747,#14748,#14749,#14750),(#14751,#14752,#14753,#14754,#14755,
#14756,#14757,#14758,#14759,#14760,#14761,#14762,#14763,#14764,#14765,#14766,
#14767,#14768,#14769,#14770,#14771,#14772,#14773,#14774,#14775,#14776,#14777,
#14778,#14779,#14780,#14781,#14782,#14783,#14784,#14785,#14786,#14787,#14788,
#14789,#14790,#14791,#14792,#14793,#14794,#14795,#14796,#14797,#14798,#14799,
#14800,#14801,#14802,#14803,#14804,#14805,#14806,#14807,#14808,#14809,#14810,
#14811,#14812,#14813,#14814,#14815,#14816,#14817,#14818,#14819,#14820,#14821,
#14822,#14823,#14824,#14825,#14826,#14827,#14828,#14829,#14830,#14831),
(#14832,#14833,#14834,#14835,#14836,#14837,#14838,#14839,#14840,#14841,
#14842,#14843,#14844,#14845,#14846,#14847,#14848,#14849,#14850,#14851,#14852,
#14853,#14854,#14855,#14856,#14857,#14858,#14859,#14860,#14861,#14862,#14863,
#14864,#14865,#14866,#14867,#14868,#14869,#14870,#14871,#14872,#14873,#14874,
#14875,#14876,#14877,#14878,#14879,#14880,#14881,#14882,#14883,#14884,#14885,
#14886,#14887,#14888,#14889,#14890,#14891,#14892,#14893,#14894,#14895,#14896,
#14897,#14898,#14899,#14900,#14901,#14902,#14903,#14904,#14905,#14906,#14907,
#14908,#14909,#14910,#14911,#14912),(#14913,#14914,#14915,#14916,#14917,
#14918,#14919,#14920,#14921,#14922,#14923,#14924,#14925,#14926,#14927,#14928,
#14929,#14930,#14931,#14932,#14933,#14934,#14935,#14936,#14937,#14938,#14939,
#14940,#14941,#14942,#14943,#14944,#14945,#14946,#14947,#14948,#14949,#14950,
#14951,#14952,#14953,#14954,#14955,#14956,#14957,#14958,#14959,#14960,#14961,
#14962,#14963,#14964,#14965,#14966,#14967,#14968,#14969,#14970,#14971,#14972,
#14973,#14974,#14975,#14976,#14977,#14978,#14979,#14980,#14981,#14982,#14983,
#14984,#14985,#14986,#14987,#14988,#14989,#14990,#14991,#14992,#14993),
(#14994,#14995,#14996,#14997,#14998,#14999,#15000,#15001,#15002,#15003,
#15004,#15005,#15006,#15007,#15008,#15009,#15010,#15011,#15012,#15013,#15014,
#15015,#15016,#15017,#15018,#15019,#15020,#15021,#15022,#15023,#15024,#15025,
#15026,#15027,#15028,#15029,#15030,#15031,#15032,#15033,#15034,#15035,#15036,
#15037,#15038,#15039,#15040,#15041,#15042,#15043,#15044,#15045,#15046,#15047,
#15048,#15049,#15050,#15051,#15052,#15053,#15054,#15055,#15056,#15057,#15058,
#15059,#15060,#15061,#15062,#15063,#15064,#15065,#15066,#15067,#15068,#15069,
#15070,#15071,#15072,#15073,#15074),(#15075,#15076,#15077,#15078,#15079,
#15080,#15081,#15082,#15083,#15084,#15085,#15086,#15087,#15088,#15089,#15090,
#15091,#15092,#15093,#15094,#15095,#15096,#15097,#15098,#15099,#15100,#15101,
#15102,#15103,#15104,#15105,#15106,#15107,#15108,#15109,#15110,#15111,#15112,
#15113,#15114,#15115,#15116,#15117,#15118,#15119,#15120,#15121,#15122,#15123,
#15124,#15125,#15126,#15127,#15128,#15129,#15130,#15131,#15132,#15133,#15134,
#15135,#15136,#15137,#15138,#15139,#15140,#15141,#15142,#15143,#15144,#15145,
#15146,#15147,#15148,#15149,#15150,#15151,#15152,#15153,#15154,#15155),
(#15156,#15157,#15158,#15159,#15160,#15161,#15162,#15163,#15164,#15165,
#15166,#15167,#15168,#15169,#15170,#15171,#15172,#15173,#15174,#15175,#15176,
#15177,#15178,#15179,#15180,#15181,#15182,#15183,#15184,#15185,#15186,#15187,
#15188,#15189,#15190,#15191,#15192,#15193,#15194,#15195,#15196,#15197,#15198,
#15199,#15200,#15201,#15202,#15203,#15204,#15205,#15206,#15207,#15208,#15209,
#15210,#15211,#15212,#15213,#15214,#15215,#15216,#15217,#15218,#15219,#15220,
#15221,#15222,#15223,#15224,#15225,#15226,#15227,#15228,#15229,#15230,#15231,
#15232,#15233,#15234,#15235,#15236)),.UNSPECIFIED.,.T.,.F.,.F.,(4,1,1,1,
1,1,1,4),(4,1,1,1,1,1,1,1,1,1,1,1,1,1,1,1,1,1,1,1,1,1,1,1,1,1,1,1,1,1,1,
1,1,1,1,1,1,1,1,1,1,1,1,1,1,1,1,1,1,1,1,1,1,1,1,1,1,1,1,1,1,1,1,1,1,1,1,
1,1,1,1,1,1,1,1,1,1,1,4),(-3.14159265358979,-2.24399475256414,-1.34639685153848,
-0.448798950512828,0.448798950512828,1.34639685153848,2.24399475256414,
3.14159265358979),(0.,0.00892857142857143,0.0178571428571429,0.0357142857142857,
0.0535714285714286,0.0714285714285714,0.0892857142857143,0.107142857142857,
0.125,0.142857142857143,0.158730158730159,0.174603174603175,0.19047619047619,
0.202380952380952,0.214285714285714,0.220238095238095,0.226190476190476,
0.238095238095238,0.25,0.261904761904762,0.273809523809524,0.285714285714286,
0.297619047619048,0.30952380952381,0.321428571428571,0.333333333333333,
0.349206349206349,0.365079365079365,0.376984126984127,0.380952380952381,
0.392857142857143,0.404761904761905,0.416666666666667,0.428571428571429,
0.446428571428571,0.464285714285714,0.476190476190476,0.485119047619048,
0.5,0.508928571428571,0.517857142857143,0.535714285714286,0.553571428571429,
0.571428571428571,0.589285714285714,0.607142857142857,0.625,0.642857142857143,
0.651785714285714,0.654761904761905,0.666666666666667,0.678571428571428,
0.696428571428571,0.705357142857143,0.714285714285714,0.726190476190476,
0.738095238095238,0.75,0.761904761904762,0.773809523809524,0.785714285714286,
0.797619047619047,0.803571428571428,0.806547619047619,0.809523809523809,
0.821428571428571,0.833333333333333,0.845238095238095,0.857142857142857,
0.866071428571429,0.875,0.892857142857143,0.910714285714286,0.928571428571429,
0.946428571428571,0.964285714285714,0.982142857142857,0.991071428571429,
1.),.UNSPECIFIED.);
#517=SHAPE_REPRESENTATION_RELATIONSHIP('SRR','None',#17260,#564);
#518=SHAPE_REPRESENTATION_RELATIONSHIP('SRR','None',#17261,#565);
#519=SHAPE_REPRESENTATION_RELATIONSHIP('SRR','None',#17262,#566);
#520=SHAPE_REPRESENTATION_RELATIONSHIP('SRR','None',#17263,#567);
#521=SHAPE_REPRESENTATION_RELATIONSHIP('SRR','None',#17264,#568);
#522=SHAPE_REPRESENTATION_RELATIONSHIP('SRR','None',#17265,#569);
#523=SHAPE_REPRESENTATION_RELATIONSHIP('SRR','None',#17266,#570);
#524=SHAPE_REPRESENTATION_RELATIONSHIP('SRR','None',#17267,#571);
#525=SHAPE_REPRESENTATION_RELATIONSHIP('SRR','None',#17268,#572);
#526=SHAPE_REPRESENTATION_RELATIONSHIP('SRR','None',#17269,#573);
#527=SHAPE_REPRESENTATION_RELATIONSHIP('SRR','None',#17270,#574);
#528=SHAPE_REPRESENTATION_RELATIONSHIP('SRR','None',#17271,#575);
#529=SHAPE_REPRESENTATION_RELATIONSHIP('SRR','None',#17272,#576);
#530=SHAPE_REPRESENTATION_RELATIONSHIP('SRR','None',#17273,#577);
#531=SHAPE_REPRESENTATION_RELATIONSHIP('SRR','None',#17274,#578);
#532=SHAPE_REPRESENTATION_RELATIONSHIP('SRR','None',#17275,#579);
#533=SHAPE_REPRESENTATION_RELATIONSHIP('SRR','None',#17276,#580);
#534=SHAPE_REPRESENTATION_RELATIONSHIP('SRR','None',#17277,#581);
#535=SHAPE_REPRESENTATION_RELATIONSHIP('SRR','None',#17278,#582);
#536=SHAPE_REPRESENTATION_RELATIONSHIP('SRR','None',#17279,#583);
#537=SHAPE_REPRESENTATION_RELATIONSHIP('SRR','None',#17280,#584);
#538=SHAPE_REPRESENTATION_RELATIONSHIP('SRR','None',#17281,#585);
#539=SHAPE_REPRESENTATION_RELATIONSHIP('SRR','None',#17282,#586);
#540=SHAPE_REPRESENTATION_RELATIONSHIP('SRR','None',#17283,#587);
#541=SHAPE_REPRESENTATION_RELATIONSHIP('SRR','None',#17285,#588);
#542=SHAPE_REPRESENTATION_RELATIONSHIP('SRR','None',#17286,#589);
#543=SHAPE_REPRESENTATION_RELATIONSHIP('SRR','None',#17287,#590);
#544=SHAPE_REPRESENTATION_RELATIONSHIP('SRR','None',#17288,#591);
#545=SHAPE_REPRESENTATION_RELATIONSHIP('SRR','None',#17289,#592);
#546=SHAPE_REPRESENTATION_RELATIONSHIP('SRR','None',#17290,#593);
#547=SHAPE_REPRESENTATION_RELATIONSHIP('SRR','None',#17291,#594);
#548=SHAPE_REPRESENTATION_RELATIONSHIP('SRR','None',#17292,#595);
#549=SHAPE_REPRESENTATION_RELATIONSHIP('SRR','None',#17294,#596);
#550=SHAPE_REPRESENTATION_RELATIONSHIP('SRR','None',#17295,#597);
#551=SHAPE_REPRESENTATION_RELATIONSHIP('SRR','None',#17296,#598);
#552=SHAPE_REPRESENTATION_RELATIONSHIP('SRR','None',#17297,#599);
#553=SHAPE_REPRESENTATION_RELATIONSHIP('SRR','None',#17298,#600);
#554=SHAPE_REPRESENTATION_RELATIONSHIP('SRR','None',#17299,#601);
#555=SHAPE_REPRESENTATION_RELATIONSHIP('SRR','None',#17300,#602);
#556=SHAPE_REPRESENTATION_RELATIONSHIP('SRR','None',#17302,#603);
#557=SHAPE_REPRESENTATION_RELATIONSHIP('SRR','None',#17303,#604);
#558=SHAPE_REPRESENTATION_RELATIONSHIP('SRR','None',#17304,#605);
#559=SHAPE_REPRESENTATION_RELATIONSHIP('SRR','None',#17305,#606);
#560=SHAPE_REPRESENTATION_RELATIONSHIP('SRR','None',#17306,#607);
#561=SHAPE_REPRESENTATION_RELATIONSHIP('SRR','None',#17307,#608);
#562=SHAPE_REPRESENTATION_RELATIONSHIP('SRR','None',#17308,#609);
#563=SHAPE_REPRESENTATION_RELATIONSHIP('SRR','None',#17309,#610);
#564=ADVANCED_BREP_SHAPE_REPRESENTATION('',(#665),#16996);
#565=ADVANCED_BREP_SHAPE_REPRESENTATION('',(#666),#16997);
#566=ADVANCED_BREP_SHAPE_REPRESENTATION('',(#667),#16998);
#567=ADVANCED_BREP_SHAPE_REPRESENTATION('',(#668),#16999);
#568=ADVANCED_BREP_SHAPE_REPRESENTATION('',(#669),#17000);
#569=ADVANCED_BREP_SHAPE_REPRESENTATION('',(#670),#17001);
#570=ADVANCED_BREP_SHAPE_REPRESENTATION('',(#671),#17002);
#571=ADVANCED_BREP_SHAPE_REPRESENTATION('',(#672),#17003);
#572=ADVANCED_BREP_SHAPE_REPRESENTATION('',(#673),#17004);
#573=ADVANCED_BREP_SHAPE_REPRESENTATION('',(#674),#17005);
#574=ADVANCED_BREP_SHAPE_REPRESENTATION('',(#675),#17006);
#575=ADVANCED_BREP_SHAPE_REPRESENTATION('',(#676),#17007);
#576=ADVANCED_BREP_SHAPE_REPRESENTATION('',(#677),#17008);
#577=ADVANCED_BREP_SHAPE_REPRESENTATION('',(#678),#17009);
#578=ADVANCED_BREP_SHAPE_REPRESENTATION('',(#679),#17010);
#579=ADVANCED_BREP_SHAPE_REPRESENTATION('',(#680),#17011);
#580=ADVANCED_BREP_SHAPE_REPRESENTATION('',(#681),#17012);
#581=ADVANCED_BREP_SHAPE_REPRESENTATION('',(#682),#17013);
#582=ADVANCED_BREP_SHAPE_REPRESENTATION('',(#683),#17014);
#583=ADVANCED_BREP_SHAPE_REPRESENTATION('',(#684),#17015);
#584=ADVANCED_BREP_SHAPE_REPRESENTATION('',(#685),#17016);
#585=ADVANCED_BREP_SHAPE_REPRESENTATION('',(#686),#17017);
#586=ADVANCED_BREP_SHAPE_REPRESENTATION('',(#687),#17018);
#587=ADVANCED_BREP_SHAPE_REPRESENTATION('',(#477),#17019);
#588=ADVANCED_BREP_SHAPE_REPRESENTATION('',(#688),#17021);
#589=ADVANCED_BREP_SHAPE_REPRESENTATION('',(#689),#17022);
#590=ADVANCED_BREP_SHAPE_REPRESENTATION('',(#690,#691,#692,#693,#694,#695,
#696),#17023);
#591=ADVANCED_BREP_SHAPE_REPRESENTATION('',(#697),#17024);
#592=ADVANCED_BREP_SHAPE_REPRESENTATION('',(#698,#699),#17025);
#593=ADVANCED_BREP_SHAPE_REPRESENTATION('',(#478),#17026);
#594=ADVANCED_BREP_SHAPE_REPRESENTATION('',(#479),#17027);
#595=ADVANCED_BREP_SHAPE_REPRESENTATION('',(#700),#17028);
#596=ADVANCED_BREP_SHAPE_REPRESENTATION('',(#701),#17030);
#597=ADVANCED_BREP_SHAPE_REPRESENTATION('',(#702),#17031);
#598=ADVANCED_BREP_SHAPE_REPRESENTATION('',(#703),#17032);
#599=ADVANCED_BREP_SHAPE_REPRESENTATION('',(#704),#17033);
#600=ADVANCED_BREP_SHAPE_REPRESENTATION('',(#705),#17034);
#601=ADVANCED_BREP_SHAPE_REPRESENTATION('',(#706),#17035);
#602=ADVANCED_BREP_SHAPE_REPRESENTATION('',(#480),#17036);
#603=ADVANCED_BREP_SHAPE_REPRESENTATION('',(#707),#17038);
#604=ADVANCED_BREP_SHAPE_REPRESENTATION('',(#708),#17039);
#605=ADVANCED_BREP_SHAPE_REPRESENTATION('',(#709),#17040);
#606=ADVANCED_BREP_SHAPE_REPRESENTATION('',(#710),#17041);
#607=ADVANCED_BREP_SHAPE_REPRESENTATION('',(#711),#17042);
#608=ADVANCED_BREP_SHAPE_REPRESENTATION('',(#712),#17043);
#609=ADVANCED_BREP_SHAPE_REPRESENTATION('',(#713),#17044);
#610=ADVANCED_BREP_SHAPE_REPRESENTATION('',(#714),#17045);
#611=STYLED_ITEM('',(#17570),#665);
#612=STYLED_ITEM('',(#17577),#666);
#613=STYLED_ITEM('',(#17577),#667);
#614=STYLED_ITEM('',(#17584),#668);
#615=STYLED_ITEM('',(#17591),#669);
#616=STYLED_ITEM('',(#17591),#670);
#617=STYLED_ITEM('',(#17591),#671);
#618=STYLED_ITEM('',(#17591),#672);
#619=STYLED_ITEM('',(#17591),#673);
#620=STYLED_ITEM('',(#17591),#674);
#621=STYLED_ITEM('',(#17591),#675);
#622=STYLED_ITEM('',(#17591),#676);
#623=STYLED_ITEM('',(#17591),#677);
#624=STYLED_ITEM('',(#17591),#678);
#625=STYLED_ITEM('',(#17591),#679);
#626=STYLED_ITEM('',(#17591),#680);
#627=STYLED_ITEM('',(#17605),#681);
#628=STYLED_ITEM('',(#17591),#682);
#629=STYLED_ITEM('',(#17591),#683);
#630=STYLED_ITEM('',(#17591),#684);
#631=STYLED_ITEM('',(#17591),#685);
#632=STYLED_ITEM('',(#17591),#686);
#633=STYLED_ITEM('',(#17591),#687);
#634=STYLED_ITEM('',(#17598),#477);
#635=STYLED_ITEM('',(#17591),#688);
#636=STYLED_ITEM('',(#17591),#689);
#637=STYLED_ITEM('',(#17591),#690);
#638=STYLED_ITEM('',(#17591),#691);
#639=STYLED_ITEM('',(#17591),#692);
#640=STYLED_ITEM('',(#17591),#693);
#641=STYLED_ITEM('',(#17591),#694);
#642=STYLED_ITEM('',(#17591),#695);
#643=STYLED_ITEM('',(#17591),#696);
#644=STYLED_ITEM('',(#17591),#697);
#645=STYLED_ITEM('',(#17591),#698);
#646=STYLED_ITEM('',(#17591),#699);
#647=STYLED_ITEM('',(#17598),#478);
#648=STYLED_ITEM('',(#17598),#479);
#649=STYLED_ITEM('',(#17598),#700);
#650=STYLED_ITEM('',(#17591),#701);
#651=STYLED_ITEM('',(#17605),#702);
#652=STYLED_ITEM('',(#17584),#703);
#653=STYLED_ITEM('',(#17605),#704);
#654=STYLED_ITEM('',(#17577),#705);
#655=STYLED_ITEM('',(#17605),#706);
#656=STYLED_ITEM('',(#17598),#480);
#657=STYLED_ITEM('',(#17591),#707);
#658=STYLED_ITEM('',(#17584),#708);
#659=STYLED_ITEM('',(#17584),#709);
#660=STYLED_ITEM('',(#17584),#710);
#661=STYLED_ITEM('',(#17605),#711);
#662=STYLED_ITEM('',(#17605),#712);
#663=STYLED_ITEM('',(#17591),#713);
#664=STYLED_ITEM('',(#17598),#714);
#665=MANIFOLD_SOLID_BREP('Body1',#8166);
#666=MANIFOLD_SOLID_BREP('Body1',#8167);
#667=MANIFOLD_SOLID_BREP('Body1',#8168);
#668=MANIFOLD_SOLID_BREP('Body1',#8169);
#669=MANIFOLD_SOLID_BREP('Body1',#8170);
#670=MANIFOLD_SOLID_BREP('Body1',#8171);
#671=MANIFOLD_SOLID_BREP('Body1',#8172);
#672=MANIFOLD_SOLID_BREP('Body1',#8173);
#673=MANIFOLD_SOLID_BREP('Body1',#8174);
#674=MANIFOLD_SOLID_BREP('Body1',#8175);
#675=MANIFOLD_SOLID_BREP('Body1',#8176);
#676=MANIFOLD_SOLID_BREP('Body1',#8177);
#677=MANIFOLD_SOLID_BREP('Body1',#8178);
#678=MANIFOLD_SOLID_BREP('Body1',#8179);
#679=MANIFOLD_SOLID_BREP('Body1',#8180);
#680=MANIFOLD_SOLID_BREP('Body1',#8181);
#681=MANIFOLD_SOLID_BREP('Body1',#8182);
#682=MANIFOLD_SOLID_BREP('Body1',#8183);
#683=MANIFOLD_SOLID_BREP('Body1',#8184);
#684=MANIFOLD_SOLID_BREP('Body1',#8185);
#685=MANIFOLD_SOLID_BREP('Body1',#8186);
#686=MANIFOLD_SOLID_BREP('Body1',#8187);
#687=MANIFOLD_SOLID_BREP('Body1',#8188);
#688=MANIFOLD_SOLID_BREP('Body1',#8191);
#689=MANIFOLD_SOLID_BREP('Body1',#8192);
#690=MANIFOLD_SOLID_BREP('Body1',#8193);
#691=MANIFOLD_SOLID_BREP('Body2',#8194);
#692=MANIFOLD_SOLID_BREP('Body3',#8195);
#693=MANIFOLD_SOLID_BREP('Body4',#8196);
#694=MANIFOLD_SOLID_BREP('Body5',#8197);
#695=MANIFOLD_SOLID_BREP('Body6',#8198);
#696=MANIFOLD_SOLID_BREP('Body7',#8199);
#697=MANIFOLD_SOLID_BREP('Continuous crown cage',#8200);
#698=MANIFOLD_SOLID_BREP('Body1',#8201);
#699=MANIFOLD_SOLID_BREP('Body2',#8202);
#700=MANIFOLD_SOLID_BREP('Body1',#8207);
#701=MANIFOLD_SOLID_BREP('Body1',#8208);
#702=MANIFOLD_SOLID_BREP('Body1',#8209);
#703=MANIFOLD_SOLID_BREP('Body1',#8210);
#704=MANIFOLD_SOLID_BREP('Body1',#8211);
#705=MANIFOLD_SOLID_BREP('Body1',#8212);
#706=MANIFOLD_SOLID_BREP('Body1',#8213);
#707=MANIFOLD_SOLID_BREP('Body1',#8216);
#708=MANIFOLD_SOLID_BREP('Body1',#8217);
#709=MANIFOLD_SOLID_BREP('Body1',#8218);
#710=MANIFOLD_SOLID_BREP('Body1',#8219);
#711=MANIFOLD_SOLID_BREP('Body1',#8220);
#712=MANIFOLD_SOLID_BREP('Body1',#8221);
#713=MANIFOLD_SOLID_BREP('Body1',#8222);
#714=MANIFOLD_SOLID_BREP('Body1',#8223);
#715=FACE_BOUND('',#1689,.T.);
#716=FACE_BOUND('',#1690,.T.);
#717=FACE_BOUND('',#1691,.T.);
#718=FACE_BOUND('',#1692,.T.);
#719=FACE_BOUND('',#1693,.T.);
#720=FACE_BOUND('',#1694,.T.);
#721=FACE_BOUND('',#1695,.T.);
#722=FACE_BOUND('',#1696,.T.);
#723=FACE_BOUND('',#1697,.T.);
#724=FACE_BOUND('',#1698,.T.);
#725=FACE_BOUND('',#1700,.T.);
#726=FACE_BOUND('',#1701,.T.);
#727=FACE_BOUND('',#1702,.T.);
#728=FACE_BOUND('',#1703,.T.);
#729=FACE_BOUND('',#1704,.T.);
#730=FACE_BOUND('',#1705,.T.);
#731=FACE_BOUND('',#1706,.T.);
#732=FACE_BOUND('',#1707,.T.);
#733=FACE_BOUND('',#1708,.T.);
#734=FACE_BOUND('',#1709,.T.);
#735=FACE_BOUND('',#1729,.T.);
#736=FACE_BOUND('',#1730,.T.);
#737=FACE_BOUND('',#1731,.T.);
#738=FACE_BOUND('',#1732,.T.);
#739=FACE_BOUND('',#1733,.T.);
#740=FACE_BOUND('',#1734,.T.);
#741=FACE_BOUND('',#1735,.T.);
#742=FACE_BOUND('',#1736,.T.);
#743=FACE_BOUND('',#1756,.T.);
#744=FACE_BOUND('',#1757,.T.);
#745=FACE_BOUND('',#1758,.T.);
#746=FACE_BOUND('',#1759,.T.);
#747=FACE_BOUND('',#1760,.T.);
#748=FACE_BOUND('',#1761,.T.);
#749=FACE_BOUND('',#1762,.T.);
#750=FACE_BOUND('',#1763,.T.);
#751=FACE_BOUND('',#1772,.T.);
#752=FACE_BOUND('',#1774,.T.);
#753=FACE_BOUND('',#1778,.T.);
#754=FACE_BOUND('',#1779,.T.);
#755=FACE_BOUND('',#1780,.T.);
#756=FACE_BOUND('',#1781,.T.);
#757=FACE_BOUND('',#1782,.T.);
#758=FACE_BOUND('',#1785,.T.);
#759=FACE_BOUND('',#1786,.T.);
#760=FACE_BOUND('',#1787,.T.);
#761=FACE_BOUND('',#1788,.T.);
#762=FACE_BOUND('',#1789,.T.);
#763=FACE_BOUND('',#1793,.T.);
#764=FACE_BOUND('',#1794,.T.);
#765=FACE_BOUND('',#1801,.T.);
#766=FACE_BOUND('',#1805,.T.);
#767=FACE_BOUND('',#1806,.T.);
#768=FACE_BOUND('',#1807,.T.);
#769=FACE_BOUND('',#1808,.T.);
#770=FACE_BOUND('',#1809,.T.);
#771=FACE_BOUND('',#1811,.T.);
#772=FACE_BOUND('',#1812,.T.);
#773=FACE_BOUND('',#1813,.T.);
#774=FACE_BOUND('',#1814,.T.);
#775=FACE_BOUND('',#1815,.T.);
#776=FACE_BOUND('',#1822,.T.);
#777=FACE_BOUND('',#1826,.T.);
#778=FACE_BOUND('',#1827,.T.);
#779=FACE_BOUND('',#1828,.T.);
#780=FACE_BOUND('',#1829,.T.);
#781=FACE_BOUND('',#1830,.T.);
#782=FACE_BOUND('',#1832,.T.);
#783=FACE_BOUND('',#1833,.T.);
#784=FACE_BOUND('',#1834,.T.);
#785=FACE_BOUND('',#1835,.T.);
#786=FACE_BOUND('',#1836,.T.);
#787=FACE_BOUND('',#1845,.T.);
#788=FACE_BOUND('',#1847,.T.);
#789=FACE_BOUND('',#1851,.T.);
#790=FACE_BOUND('',#1852,.T.);
#791=FACE_BOUND('',#1853,.T.);
#792=FACE_BOUND('',#1854,.T.);
#793=FACE_BOUND('',#1855,.T.);
#794=FACE_BOUND('',#1858,.T.);
#795=FACE_BOUND('',#1859,.T.);
#796=FACE_BOUND('',#1860,.T.);
#797=FACE_BOUND('',#1861,.T.);
#798=FACE_BOUND('',#1862,.T.);
#799=FACE_BOUND('',#1866,.T.);
#800=FACE_BOUND('',#1867,.T.);
#801=FACE_BOUND('',#1874,.T.);
#802=FACE_BOUND('',#1878,.T.);
#803=FACE_BOUND('',#1879,.T.);
#804=FACE_BOUND('',#1880,.T.);
#805=FACE_BOUND('',#1881,.T.);
#806=FACE_BOUND('',#1882,.T.);
#807=FACE_BOUND('',#1884,.T.);
#808=FACE_BOUND('',#1885,.T.);
#809=FACE_BOUND('',#1886,.T.);
#810=FACE_BOUND('',#1887,.T.);
#811=FACE_BOUND('',#1888,.T.);
#812=FACE_BOUND('',#1895,.T.);
#813=FACE_BOUND('',#1899,.T.);
#814=FACE_BOUND('',#1900,.T.);
#815=FACE_BOUND('',#1901,.T.);
#816=FACE_BOUND('',#1902,.T.);
#817=FACE_BOUND('',#1903,.T.);
#818=FACE_BOUND('',#1905,.T.);
#819=FACE_BOUND('',#1906,.T.);
#820=FACE_BOUND('',#1907,.T.);
#821=FACE_BOUND('',#1908,.T.);
#822=FACE_BOUND('',#1909,.T.);
#823=FACE_BOUND('',#1918,.T.);
#824=FACE_BOUND('',#1920,.T.);
#825=FACE_BOUND('',#1925,.T.);
#826=FACE_BOUND('',#1926,.T.);
#827=FACE_BOUND('',#1927,.T.);
#828=FACE_BOUND('',#1928,.T.);
#829=FACE_BOUND('',#1929,.T.);
#830=FACE_BOUND('',#1932,.T.);
#831=FACE_BOUND('',#1933,.T.);
#832=FACE_BOUND('',#1934,.T.);
#833=FACE_BOUND('',#1935,.T.);
#834=FACE_BOUND('',#1936,.T.);
#835=FACE_BOUND('',#1939,.T.);
#836=FACE_BOUND('',#1940,.T.);
#837=FACE_BOUND('',#1947,.T.);
#838=FACE_BOUND('',#1951,.T.);
#839=FACE_BOUND('',#1952,.T.);
#840=FACE_BOUND('',#1953,.T.);
#841=FACE_BOUND('',#1954,.T.);
#842=FACE_BOUND('',#1955,.T.);
#843=FACE_BOUND('',#1957,.T.);
#844=FACE_BOUND('',#1958,.T.);
#845=FACE_BOUND('',#1959,.T.);
#846=FACE_BOUND('',#1960,.T.);
#847=FACE_BOUND('',#1961,.T.);
#848=FACE_BOUND('',#1968,.T.);
#849=FACE_BOUND('',#1972,.T.);
#850=FACE_BOUND('',#1973,.T.);
#851=FACE_BOUND('',#1974,.T.);
#852=FACE_BOUND('',#1975,.T.);
#853=FACE_BOUND('',#1976,.T.);
#854=FACE_BOUND('',#1978,.T.);
#855=FACE_BOUND('',#1979,.T.);
#856=FACE_BOUND('',#1980,.T.);
#857=FACE_BOUND('',#1981,.T.);
#858=FACE_BOUND('',#1982,.T.);
#859=FACE_BOUND('',#1991,.T.);
#860=FACE_BOUND('',#1993,.T.);
#861=FACE_BOUND('',#1998,.T.);
#862=FACE_BOUND('',#1999,.T.);
#863=FACE_BOUND('',#2000,.T.);
#864=FACE_BOUND('',#2001,.T.);
#865=FACE_BOUND('',#2002,.T.);
#866=FACE_BOUND('',#2005,.T.);
#867=FACE_BOUND('',#2006,.T.);
#868=FACE_BOUND('',#2007,.T.);
#869=FACE_BOUND('',#2008,.T.);
#870=FACE_BOUND('',#2009,.T.);
#871=FACE_BOUND('',#2012,.T.);
#872=FACE_BOUND('',#2013,.T.);
#873=FACE_BOUND('',#2020,.T.);
#874=FACE_BOUND('',#2024,.T.);
#875=FACE_BOUND('',#2025,.T.);
#876=FACE_BOUND('',#2026,.T.);
#877=FACE_BOUND('',#2027,.T.);
#878=FACE_BOUND('',#2028,.T.);
#879=FACE_BOUND('',#2030,.T.);
#880=FACE_BOUND('',#2031,.T.);
#881=FACE_BOUND('',#2032,.T.);
#882=FACE_BOUND('',#2033,.T.);
#883=FACE_BOUND('',#2034,.T.);
#884=FACE_BOUND('',#2041,.T.);
#885=FACE_BOUND('',#2045,.T.);
#886=FACE_BOUND('',#2046,.T.);
#887=FACE_BOUND('',#2047,.T.);
#888=FACE_BOUND('',#2048,.T.);
#889=FACE_BOUND('',#2049,.T.);
#890=FACE_BOUND('',#2051,.T.);
#891=FACE_BOUND('',#2052,.T.);
#892=FACE_BOUND('',#2053,.T.);
#893=FACE_BOUND('',#2054,.T.);
#894=FACE_BOUND('',#2055,.T.);
#895=FACE_BOUND('',#2060,.T.);
#896=FACE_BOUND('',#2064,.T.);
#897=FACE_BOUND('',#2067,.T.);
#898=FACE_BOUND('',#2068,.T.);
#899=FACE_BOUND('',#2071,.T.);
#900=FACE_BOUND('',#2072,.T.);
#901=FACE_BOUND('',#2075,.T.);
#902=FACE_BOUND('',#2076,.T.);
#903=FACE_BOUND('',#2078,.T.);
#904=FACE_BOUND('',#2079,.T.);
#905=FACE_BOUND('',#2103,.T.);
#906=FACE_BOUND('',#2121,.T.);
#907=FACE_BOUND('',#2124,.T.);
#908=FACE_BOUND('',#2129,.T.);
#909=FACE_BOUND('',#2134,.T.);
#910=FACE_BOUND('',#2159,.T.);
#911=FACE_BOUND('',#2162,.T.);
#912=FACE_BOUND('',#2165,.T.);
#913=FACE_BOUND('',#2168,.T.);
#914=FACE_BOUND('',#2171,.T.);
#915=FACE_BOUND('',#2187,.T.);
#916=FACE_BOUND('',#2195,.T.);
#917=FACE_BOUND('',#2218,.T.);
#918=FACE_BOUND('',#2220,.T.);
#919=FACE_BOUND('',#2229,.T.);
#920=FACE_BOUND('',#2231,.T.);
#921=FACE_BOUND('',#2235,.T.);
#922=FACE_BOUND('',#2237,.T.);
#923=FACE_BOUND('',#2242,.T.);
#924=FACE_BOUND('',#2244,.T.);
#925=FACE_BOUND('',#2249,.T.);
#926=FACE_BOUND('',#2251,.T.);
#927=FACE_BOUND('',#2253,.T.);
#928=FACE_BOUND('',#2255,.T.);
#929=FACE_BOUND('',#2260,.T.);
#930=FACE_BOUND('',#2263,.T.);
#931=FACE_BOUND('',#2267,.T.);
#932=FACE_BOUND('',#2271,.T.);
#933=FACE_BOUND('',#2273,.T.);
#934=FACE_BOUND('',#2277,.T.);
#935=FACE_BOUND('',#2279,.T.);
#936=FACE_BOUND('',#2285,.T.);
#937=FACE_BOUND('',#2304,.T.);
#938=FACE_BOUND('',#2306,.T.);
#939=FACE_BOUND('',#2310,.T.);
#940=FACE_BOUND('',#2317,.T.);
#941=FACE_BOUND('',#2320,.T.);
#942=FACE_BOUND('',#2324,.T.);
#943=FACE_BOUND('',#2328,.T.);
#944=FACE_BOUND('',#2330,.T.);
#945=FACE_BOUND('',#2334,.T.);
#946=FACE_BOUND('',#2336,.T.);
#947=FACE_BOUND('',#2343,.T.);
#948=FACE_BOUND('',#2345,.T.);
#949=FACE_BOUND('',#2352,.T.);
#950=FACE_BOUND('',#2354,.T.);
#951=FACE_BOUND('',#2374,.T.);
#952=PLANE('',#8775);
#953=PLANE('',#8776);
#954=PLANE('',#8777);
#955=PLANE('',#8778);
#956=PLANE('',#8779);
#957=PLANE('',#8780);
#958=PLANE('',#8782);
#959=PLANE('',#8783);
#960=PLANE('',#8784);
#961=PLANE('',#8785);
#962=PLANE('',#8786);
#963=PLANE('',#8787);
#964=PLANE('',#8789);
#965=PLANE('',#8790);
#966=PLANE('',#8791);
#967=PLANE('',#8792);
#968=PLANE('',#8793);
#969=PLANE('',#8794);
#970=PLANE('',#8814);
#971=PLANE('',#8821);
#972=PLANE('',#8822);
#973=PLANE('',#8827);
#974=PLANE('',#8828);
#975=PLANE('',#8833);
#976=PLANE('',#8834);
#977=PLANE('',#8839);
#978=PLANE('',#8840);
#979=PLANE('',#8841);
#980=PLANE('',#8842);
#981=PLANE('',#8843);
#982=PLANE('',#8844);
#983=PLANE('',#8845);
#984=PLANE('',#8868);
#985=PLANE('',#8869);
#986=PLANE('',#8870);
#987=PLANE('',#8871);
#988=PLANE('',#8872);
#989=PLANE('',#8873);
#990=PLANE('',#8874);
#991=PLANE('',#8875);
#992=PLANE('',#8876);
#993=PLANE('',#8877);
#994=PLANE('',#8894);
#995=PLANE('',#8901);
#996=PLANE('',#8902);
#997=PLANE('',#8919);
#998=PLANE('',#8926);
#999=PLANE('',#8927);
#1000=PLANE('',#8950);
#1001=PLANE('',#8951);
#1002=PLANE('',#8952);
#1003=PLANE('',#8953);
#1004=PLANE('',#8954);
#1005=PLANE('',#8955);
#1006=PLANE('',#8956);
#1007=PLANE('',#8957);
#1008=PLANE('',#8958);
#1009=PLANE('',#8959);
#1010=PLANE('',#8976);
#1011=PLANE('',#8983);
#1012=PLANE('',#8984);
#1013=PLANE('',#9001);
#1014=PLANE('',#9008);
#1015=PLANE('',#9009);
#1016=PLANE('',#9032);
#1017=PLANE('',#9033);
#1018=PLANE('',#9034);
#1019=PLANE('',#9035);
#1020=PLANE('',#9036);
#1021=PLANE('',#9037);
#1022=PLANE('',#9038);
#1023=PLANE('',#9039);
#1024=PLANE('',#9040);
#1025=PLANE('',#9041);
#1026=PLANE('',#9058);
#1027=PLANE('',#9065);
#1028=PLANE('',#9066);
#1029=PLANE('',#9083);
#1030=PLANE('',#9090);
#1031=PLANE('',#9091);
#1032=PLANE('',#9114);
#1033=PLANE('',#9115);
#1034=PLANE('',#9116);
#1035=PLANE('',#9117);
#1036=PLANE('',#9118);
#1037=PLANE('',#9119);
#1038=PLANE('',#9120);
#1039=PLANE('',#9121);
#1040=PLANE('',#9122);
#1041=PLANE('',#9123);
#1042=PLANE('',#9140);
#1043=PLANE('',#9147);
#1044=PLANE('',#9148);
#1045=PLANE('',#9165);
#1046=PLANE('',#9172);
#1047=PLANE('',#9173);
#1048=PLANE('',#9184);
#1049=PLANE('',#9191);
#1050=PLANE('',#9195);
#1051=PLANE('',#9196);
#1052=PLANE('',#9197);
#1053=PLANE('',#9198);
#1054=PLANE('',#9199);
#1055=PLANE('',#9200);
#1056=PLANE('',#9205);
#1057=PLANE('',#9206);
#1058=PLANE('',#9211);
#1059=PLANE('',#9212);
#1060=PLANE('',#9216);
#1061=PLANE('',#9217);
#1062=PLANE('',#9222);
#1063=PLANE('',#9223);
#1064=PLANE('',#9228);
#1065=PLANE('',#9229);
#1066=PLANE('',#9233);
#1067=PLANE('',#9234);
#1068=PLANE('',#9236);
#1069=PLANE('',#9244);
#1070=PLANE('',#9252);
#1071=PLANE('',#9253);
#1072=PLANE('',#9254);
#1073=PLANE('',#9255);
#1074=PLANE('',#9256);
#1075=PLANE('',#9257);
#1076=PLANE('',#9258);
#1077=PLANE('',#9259);
#1078=PLANE('',#9260);
#1079=PLANE('',#9276);
#1080=PLANE('',#9279);
#1081=PLANE('',#9291);
#1082=PLANE('',#9300);
#1083=PLANE('',#9331);
#1084=PLANE('',#9336);
#1085=PLANE('',#9341);
#1086=PLANE('',#9347);
#1087=PLANE('',#9352);
#1088=PLANE('',#9361);
#1089=PLANE('',#9365);
#1090=PLANE('',#9366);
#1091=PLANE('',#9368);
#1092=PLANE('',#9373);
#1093=PLANE('',#9376);
#1094=PLANE('',#9381);
#1095=PLANE('',#9390);
#1096=PLANE('',#9391);
#1097=PLANE('',#9392);
#1098=PLANE('',#9393);
#1099=PLANE('',#9394);
#1100=PLANE('',#9395);
#1101=PLANE('',#9396);
#1102=PLANE('',#9397);
#1103=PLANE('',#9398);
#1104=PLANE('',#9400);
#1105=PLANE('',#9408);
#1106=PLANE('',#9414);
#1107=PLANE('',#9422);
#1108=PLANE('',#9430);
#1109=PLANE('',#9431);
#1110=PLANE('',#9432);
#1111=PLANE('',#9433);
#1112=PLANE('',#9434);
#1113=PLANE('',#9435);
#1114=PLANE('',#9436);
#1115=PLANE('',#9437);
#1116=PLANE('',#9438);
#1117=PLANE('',#9444);
#1118=PLANE('',#9445);
#1119=PLANE('',#9446);
#1120=PLANE('',#9450);
#1121=PLANE('',#9451);
#1122=PLANE('',#9452);
#1123=PLANE('',#9453);
#1124=PLANE('',#9454);
#1125=PLANE('',#9460);
#1126=PLANE('',#9461);
#1127=PLANE('',#9462);
#1128=PLANE('',#9464);
#1129=PLANE('',#9465);
#1130=PLANE('',#9466);
#1131=PLANE('',#9468);
#1132=PLANE('',#9471);
#1133=PLANE('',#9479);
#1134=PLANE('',#9480);
#1135=PLANE('',#9488);
#1136=PLANE('',#9489);
#1137=PLANE('',#9491);
#1138=PLANE('',#9496);
#1139=PLANE('',#9503);
#1140=PLANE('',#9504);
#1141=PLANE('',#9506);
#1142=PLANE('',#9507);
#1143=PLANE('',#9508);
#1144=PLANE('',#9509);
#1145=PLANE('',#9514);
#1146=PLANE('',#9520);
#1147=PLANE('',#9528);
#1148=PLANE('',#9529);
#1149=PLANE('',#9537);
#1150=PLANE('',#9538);
#1151=PLANE('',#9540);
#1152=PLANE('',#9548);
#1153=PLANE('',#9556);
#1154=PLANE('',#9557);
#1155=PLANE('',#9558);
#1156=PLANE('',#9559);
#1157=PLANE('',#9560);
#1158=PLANE('',#9561);
#1159=PLANE('',#9562);
#1160=PLANE('',#9563);
#1161=PLANE('',#9564);
#1162=PLANE('',#9644);
#1163=PLANE('',#9645);
#1164=PLANE('',#9647);
#1165=PLANE('',#9648);
#1166=PLANE('',#9649);
#1167=PLANE('',#9651);
#1168=PLANE('',#9654);
#1169=PLANE('',#9662);
#1170=PLANE('',#9663);
#1171=PLANE('',#9665);
#1172=PLANE('',#9666);
#1173=PLANE('',#9667);
#1174=PLANE('',#9668);
#1175=PLANE('',#9673);
#1176=PLANE('',#9679);
#1177=PLANE('',#9687);
#1178=PLANE('',#9688);
#1179=PLANE('',#9696);
#1180=PLANE('',#9697);
#1181=PLANE('',#9699);
#1182=PLANE('',#9703);
#1183=PLANE('',#9710);
#1184=PLANE('',#9711);
#1185=PLANE('',#9713);
#1186=PLANE('',#9717);
#1187=PLANE('',#9724);
#1188=PLANE('',#9725);
#1189=PLANE('',#9727);
#1190=PLANE('',#9728);
#1191=PLANE('',#9729);
#1192=PLANE('',#9730);
#1193=PLANE('',#9731);
#1194=PLANE('',#9732);
#1195=PLANE('',#9733);
#1196=PLANE('',#9734);
#1197=PLANE('',#9735);
#1198=PLANE('',#9736);
#1199=PLANE('',#9738);
#1200=PLANE('',#9740);
#1201=PLANE('',#9741);
#1202=PLANE('',#9742);
#1203=PLANE('',#9743);
#1204=PLANE('',#9744);
#1205=PLANE('',#9745);
#1206=PLANE('',#9746);
#1207=PLANE('',#9747);
#1208=FACE_OUTER_BOUND('',#1674,.T.);
#1209=FACE_OUTER_BOUND('',#1675,.T.);
#1210=FACE_OUTER_BOUND('',#1676,.T.);
#1211=FACE_OUTER_BOUND('',#1677,.T.);
#1212=FACE_OUTER_BOUND('',#1678,.T.);
#1213=FACE_OUTER_BOUND('',#1679,.T.);
#1214=FACE_OUTER_BOUND('',#1680,.T.);
#1215=FACE_OUTER_BOUND('',#1681,.T.);
#1216=FACE_OUTER_BOUND('',#1682,.T.);
#1217=FACE_OUTER_BOUND('',#1683,.T.);
#1218=FACE_OUTER_BOUND('',#1684,.T.);
#1219=FACE_OUTER_BOUND('',#1685,.T.);
#1220=FACE_OUTER_BOUND('',#1686,.T.);
#1221=FACE_OUTER_BOUND('',#1687,.T.);
#1222=FACE_OUTER_BOUND('',#1688,.T.);
#1223=FACE_OUTER_BOUND('',#1699,.T.);
#1224=FACE_OUTER_BOUND('',#1710,.T.);
#1225=FACE_OUTER_BOUND('',#1711,.T.);
#1226=FACE_OUTER_BOUND('',#1712,.T.);
#1227=FACE_OUTER_BOUND('',#1713,.T.);
#1228=FACE_OUTER_BOUND('',#1714,.T.);
#1229=FACE_OUTER_BOUND('',#1715,.T.);
#1230=FACE_OUTER_BOUND('',#1716,.T.);
#1231=FACE_OUTER_BOUND('',#1717,.T.);
#1232=FACE_OUTER_BOUND('',#1718,.T.);
#1233=FACE_OUTER_BOUND('',#1719,.T.);
#1234=FACE_OUTER_BOUND('',#1720,.T.);
#1235=FACE_OUTER_BOUND('',#1721,.T.);
#1236=FACE_OUTER_BOUND('',#1722,.T.);
#1237=FACE_OUTER_BOUND('',#1723,.T.);
#1238=FACE_OUTER_BOUND('',#1724,.T.);
#1239=FACE_OUTER_BOUND('',#1725,.T.);
#1240=FACE_OUTER_BOUND('',#1726,.T.);
#1241=FACE_OUTER_BOUND('',#1727,.T.);
#1242=FACE_OUTER_BOUND('',#1728,.T.);
#1243=FACE_OUTER_BOUND('',#1737,.T.);
#1244=FACE_OUTER_BOUND('',#1738,.T.);
#1245=FACE_OUTER_BOUND('',#1739,.T.);
#1246=FACE_OUTER_BOUND('',#1740,.T.);
#1247=FACE_OUTER_BOUND('',#1741,.T.);
#1248=FACE_OUTER_BOUND('',#1742,.T.);
#1249=FACE_OUTER_BOUND('',#1743,.T.);
#1250=FACE_OUTER_BOUND('',#1744,.T.);
#1251=FACE_OUTER_BOUND('',#1745,.T.);
#1252=FACE_OUTER_BOUND('',#1746,.T.);
#1253=FACE_OUTER_BOUND('',#1747,.T.);
#1254=FACE_OUTER_BOUND('',#1748,.T.);
#1255=FACE_OUTER_BOUND('',#1749,.T.);
#1256=FACE_OUTER_BOUND('',#1750,.T.);
#1257=FACE_OUTER_BOUND('',#1751,.T.);
#1258=FACE_OUTER_BOUND('',#1752,.T.);
#1259=FACE_OUTER_BOUND('',#1753,.T.);
#1260=FACE_OUTER_BOUND('',#1754,.T.);
#1261=FACE_OUTER_BOUND('',#1755,.T.);
#1262=FACE_OUTER_BOUND('',#1764,.T.);
#1263=FACE_OUTER_BOUND('',#1765,.T.);
#1264=FACE_OUTER_BOUND('',#1766,.T.);
#1265=FACE_OUTER_BOUND('',#1767,.T.);
#1266=FACE_OUTER_BOUND('',#1768,.T.);
#1267=FACE_OUTER_BOUND('',#1769,.T.);
#1268=FACE_OUTER_BOUND('',#1770,.T.);
#1269=FACE_OUTER_BOUND('',#1771,.T.);
#1270=FACE_OUTER_BOUND('',#1773,.T.);
#1271=FACE_OUTER_BOUND('',#1775,.T.);
#1272=FACE_OUTER_BOUND('',#1776,.T.);
#1273=FACE_OUTER_BOUND('',#1777,.T.);
#1274=FACE_OUTER_BOUND('',#1783,.T.);
#1275=FACE_OUTER_BOUND('',#1784,.T.);
#1276=FACE_OUTER_BOUND('',#1790,.T.);
#1277=FACE_OUTER_BOUND('',#1791,.T.);
#1278=FACE_OUTER_BOUND('',#1792,.T.);
#1279=FACE_OUTER_BOUND('',#1795,.T.);
#1280=FACE_OUTER_BOUND('',#1796,.T.);
#1281=FACE_OUTER_BOUND('',#1797,.T.);
#1282=FACE_OUTER_BOUND('',#1798,.T.);
#1283=FACE_OUTER_BOUND('',#1799,.T.);
#1284=FACE_OUTER_BOUND('',#1800,.T.);
#1285=FACE_OUTER_BOUND('',#1802,.T.);
#1286=FACE_OUTER_BOUND('',#1803,.T.);
#1287=FACE_OUTER_BOUND('',#1804,.T.);
#1288=FACE_OUTER_BOUND('',#1810,.T.);
#1289=FACE_OUTER_BOUND('',#1816,.T.);
#1290=FACE_OUTER_BOUND('',#1817,.T.);
#1291=FACE_OUTER_BOUND('',#1818,.T.);
#1292=FACE_OUTER_BOUND('',#1819,.T.);
#1293=FACE_OUTER_BOUND('',#1820,.T.);
#1294=FACE_OUTER_BOUND('',#1821,.T.);
#1295=FACE_OUTER_BOUND('',#1823,.T.);
#1296=FACE_OUTER_BOUND('',#1824,.T.);
#1297=FACE_OUTER_BOUND('',#1825,.T.);
#1298=FACE_OUTER_BOUND('',#1831,.T.);
#1299=FACE_OUTER_BOUND('',#1837,.T.);
#1300=FACE_OUTER_BOUND('',#1838,.T.);
#1301=FACE_OUTER_BOUND('',#1839,.T.);
#1302=FACE_OUTER_BOUND('',#1840,.T.);
#1303=FACE_OUTER_BOUND('',#1841,.T.);
#1304=FACE_OUTER_BOUND('',#1842,.T.);
#1305=FACE_OUTER_BOUND('',#1843,.T.);
#1306=FACE_OUTER_BOUND('',#1844,.T.);
#1307=FACE_OUTER_BOUND('',#1846,.T.);
#1308=FACE_OUTER_BOUND('',#1848,.T.);
#1309=FACE_OUTER_BOUND('',#1849,.T.);
#1310=FACE_OUTER_BOUND('',#1850,.T.);
#1311=FACE_OUTER_BOUND('',#1856,.T.);
#1312=FACE_OUTER_BOUND('',#1857,.T.);
#1313=FACE_OUTER_BOUND('',#1863,.T.);
#1314=FACE_OUTER_BOUND('',#1864,.T.);
#1315=FACE_OUTER_BOUND('',#1865,.T.);
#1316=FACE_OUTER_BOUND('',#1868,.T.);
#1317=FACE_OUTER_BOUND('',#1869,.T.);
#1318=FACE_OUTER_BOUND('',#1870,.T.);
#1319=FACE_OUTER_BOUND('',#1871,.T.);
#1320=FACE_OUTER_BOUND('',#1872,.T.);
#1321=FACE_OUTER_BOUND('',#1873,.T.);
#1322=FACE_OUTER_BOUND('',#1875,.T.);
#1323=FACE_OUTER_BOUND('',#1876,.T.);
#1324=FACE_OUTER_BOUND('',#1877,.T.);
#1325=FACE_OUTER_BOUND('',#1883,.T.);
#1326=FACE_OUTER_BOUND('',#1889,.T.);
#1327=FACE_OUTER_BOUND('',#1890,.T.);
#1328=FACE_OUTER_BOUND('',#1891,.T.);
#1329=FACE_OUTER_BOUND('',#1892,.T.);
#1330=FACE_OUTER_BOUND('',#1893,.T.);
#1331=FACE_OUTER_BOUND('',#1894,.T.);
#1332=FACE_OUTER_BOUND('',#1896,.T.);
#1333=FACE_OUTER_BOUND('',#1897,.T.);
#1334=FACE_OUTER_BOUND('',#1898,.T.);
#1335=FACE_OUTER_BOUND('',#1904,.T.);
#1336=FACE_OUTER_BOUND('',#1910,.T.);
#1337=FACE_OUTER_BOUND('',#1911,.T.);
#1338=FACE_OUTER_BOUND('',#1912,.T.);
#1339=FACE_OUTER_BOUND('',#1913,.T.);
#1340=FACE_OUTER_BOUND('',#1914,.T.);
#1341=FACE_OUTER_BOUND('',#1915,.T.);
#1342=FACE_OUTER_BOUND('',#1916,.T.);
#1343=FACE_OUTER_BOUND('',#1917,.T.);
#1344=FACE_OUTER_BOUND('',#1919,.T.);
#1345=FACE_OUTER_BOUND('',#1921,.T.);
#1346=FACE_OUTER_BOUND('',#1922,.T.);
#1347=FACE_OUTER_BOUND('',#1923,.T.);
#1348=FACE_OUTER_BOUND('',#1924,.T.);
#1349=FACE_OUTER_BOUND('',#1930,.T.);
#1350=FACE_OUTER_BOUND('',#1931,.T.);
#1351=FACE_OUTER_BOUND('',#1937,.T.);
#1352=FACE_OUTER_BOUND('',#1938,.T.);
#1353=FACE_OUTER_BOUND('',#1941,.T.);
#1354=FACE_OUTER_BOUND('',#1942,.T.);
#1355=FACE_OUTER_BOUND('',#1943,.T.);
#1356=FACE_OUTER_BOUND('',#1944,.T.);
#1357=FACE_OUTER_BOUND('',#1945,.T.);
#1358=FACE_OUTER_BOUND('',#1946,.T.);
#1359=FACE_OUTER_BOUND('',#1948,.T.);
#1360=FACE_OUTER_BOUND('',#1949,.T.);
#1361=FACE_OUTER_BOUND('',#1950,.T.);
#1362=FACE_OUTER_BOUND('',#1956,.T.);
#1363=FACE_OUTER_BOUND('',#1962,.T.);
#1364=FACE_OUTER_BOUND('',#1963,.T.);
#1365=FACE_OUTER_BOUND('',#1964,.T.);
#1366=FACE_OUTER_BOUND('',#1965,.T.);
#1367=FACE_OUTER_BOUND('',#1966,.T.);
#1368=FACE_OUTER_BOUND('',#1967,.T.);
#1369=FACE_OUTER_BOUND('',#1969,.T.);
#1370=FACE_OUTER_BOUND('',#1970,.T.);
#1371=FACE_OUTER_BOUND('',#1971,.T.);
#1372=FACE_OUTER_BOUND('',#1977,.T.);
#1373=FACE_OUTER_BOUND('',#1983,.T.);
#1374=FACE_OUTER_BOUND('',#1984,.T.);
#1375=FACE_OUTER_BOUND('',#1985,.T.);
#1376=FACE_OUTER_BOUND('',#1986,.T.);
#1377=FACE_OUTER_BOUND('',#1987,.T.);
#1378=FACE_OUTER_BOUND('',#1988,.T.);
#1379=FACE_OUTER_BOUND('',#1989,.T.);
#1380=FACE_OUTER_BOUND('',#1990,.T.);
#1381=FACE_OUTER_BOUND('',#1992,.T.);
#1382=FACE_OUTER_BOUND('',#1994,.T.);
#1383=FACE_OUTER_BOUND('',#1995,.T.);
#1384=FACE_OUTER_BOUND('',#1996,.T.);
#1385=FACE_OUTER_BOUND('',#1997,.T.);
#1386=FACE_OUTER_BOUND('',#2003,.T.);
#1387=FACE_OUTER_BOUND('',#2004,.T.);
#1388=FACE_OUTER_BOUND('',#2010,.T.);
#1389=FACE_OUTER_BOUND('',#2011,.T.);
#1390=FACE_OUTER_BOUND('',#2014,.T.);
#1391=FACE_OUTER_BOUND('',#2015,.T.);
#1392=FACE_OUTER_BOUND('',#2016,.T.);
#1393=FACE_OUTER_BOUND('',#2017,.T.);
#1394=FACE_OUTER_BOUND('',#2018,.T.);
#1395=FACE_OUTER_BOUND('',#2019,.T.);
#1396=FACE_OUTER_BOUND('',#2021,.T.);
#1397=FACE_OUTER_BOUND('',#2022,.T.);
#1398=FACE_OUTER_BOUND('',#2023,.T.);
#1399=FACE_OUTER_BOUND('',#2029,.T.);
#1400=FACE_OUTER_BOUND('',#2035,.T.);
#1401=FACE_OUTER_BOUND('',#2036,.T.);
#1402=FACE_OUTER_BOUND('',#2037,.T.);
#1403=FACE_OUTER_BOUND('',#2038,.T.);
#1404=FACE_OUTER_BOUND('',#2039,.T.);
#1405=FACE_OUTER_BOUND('',#2040,.T.);
#1406=FACE_OUTER_BOUND('',#2042,.T.);
#1407=FACE_OUTER_BOUND('',#2043,.T.);
#1408=FACE_OUTER_BOUND('',#2044,.T.);
#1409=FACE_OUTER_BOUND('',#2050,.T.);
#1410=FACE_OUTER_BOUND('',#2056,.T.);
#1411=FACE_OUTER_BOUND('',#2057,.T.);
#1412=FACE_OUTER_BOUND('',#2058,.T.);
#1413=FACE_OUTER_BOUND('',#2059,.T.);
#1414=FACE_OUTER_BOUND('',#2061,.T.);
#1415=FACE_OUTER_BOUND('',#2062,.T.);
#1416=FACE_OUTER_BOUND('',#2063,.T.);
#1417=FACE_OUTER_BOUND('',#2065,.T.);
#1418=FACE_OUTER_BOUND('',#2066,.T.);
#1419=FACE_OUTER_BOUND('',#2069,.T.);
#1420=FACE_OUTER_BOUND('',#2070,.T.);
#1421=FACE_OUTER_BOUND('',#2073,.T.);
#1422=FACE_OUTER_BOUND('',#2074,.T.);
#1423=FACE_OUTER_BOUND('',#2077,.T.);
#1424=FACE_OUTER_BOUND('',#2080,.T.);
#1425=FACE_OUTER_BOUND('',#2081,.T.);
#1426=FACE_OUTER_BOUND('',#2082,.T.);
#1427=FACE_OUTER_BOUND('',#2083,.T.);
#1428=FACE_OUTER_BOUND('',#2084,.T.);
#1429=FACE_OUTER_BOUND('',#2085,.T.);
#1430=FACE_OUTER_BOUND('',#2086,.T.);
#1431=FACE_OUTER_BOUND('',#2087,.T.);
#1432=FACE_OUTER_BOUND('',#2088,.T.);
#1433=FACE_OUTER_BOUND('',#2089,.T.);
#1434=FACE_OUTER_BOUND('',#2090,.T.);
#1435=FACE_OUTER_BOUND('',#2091,.T.);
#1436=FACE_OUTER_BOUND('',#2092,.T.);
#1437=FACE_OUTER_BOUND('',#2093,.T.);
#1438=FACE_OUTER_BOUND('',#2094,.T.);
#1439=FACE_OUTER_BOUND('',#2095,.T.);
#1440=FACE_OUTER_BOUND('',#2096,.T.);
#1441=FACE_OUTER_BOUND('',#2097,.T.);
#1442=FACE_OUTER_BOUND('',#2098,.T.);
#1443=FACE_OUTER_BOUND('',#2099,.T.);
#1444=FACE_OUTER_BOUND('',#2100,.T.);
#1445=FACE_OUTER_BOUND('',#2101,.T.);
#1446=FACE_OUTER_BOUND('',#2102,.T.);
#1447=FACE_OUTER_BOUND('',#2104,.T.);
#1448=FACE_OUTER_BOUND('',#2105,.T.);
#1449=FACE_OUTER_BOUND('',#2106,.T.);
#1450=FACE_OUTER_BOUND('',#2107,.T.);
#1451=FACE_OUTER_BOUND('',#2108,.T.);
#1452=FACE_OUTER_BOUND('',#2109,.T.);
#1453=FACE_OUTER_BOUND('',#2110,.T.);
#1454=FACE_OUTER_BOUND('',#2111,.T.);
#1455=FACE_OUTER_BOUND('',#2112,.T.);
#1456=FACE_OUTER_BOUND('',#2113,.T.);
#1457=FACE_OUTER_BOUND('',#2114,.T.);
#1458=FACE_OUTER_BOUND('',#2115,.T.);
#1459=FACE_OUTER_BOUND('',#2116,.T.);
#1460=FACE_OUTER_BOUND('',#2117,.T.);
#1461=FACE_OUTER_BOUND('',#2118,.T.);
#1462=FACE_OUTER_BOUND('',#2119,.T.);
#1463=FACE_OUTER_BOUND('',#2120,.T.);
#1464=FACE_OUTER_BOUND('',#2122,.T.);
#1465=FACE_OUTER_BOUND('',#2123,.T.);
#1466=FACE_OUTER_BOUND('',#2125,.T.);
#1467=FACE_OUTER_BOUND('',#2126,.T.);
#1468=FACE_OUTER_BOUND('',#2127,.T.);
#1469=FACE_OUTER_BOUND('',#2128,.T.);
#1470=FACE_OUTER_BOUND('',#2130,.T.);
#1471=FACE_OUTER_BOUND('',#2131,.T.);
#1472=FACE_OUTER_BOUND('',#2132,.T.);
#1473=FACE_OUTER_BOUND('',#2133,.T.);
#1474=FACE_OUTER_BOUND('',#2135,.T.);
#1475=FACE_OUTER_BOUND('',#2136,.T.);
#1476=FACE_OUTER_BOUND('',#2137,.T.);
#1477=FACE_OUTER_BOUND('',#2138,.T.);
#1478=FACE_OUTER_BOUND('',#2139,.T.);
#1479=FACE_OUTER_BOUND('',#2140,.T.);
#1480=FACE_OUTER_BOUND('',#2141,.T.);
#1481=FACE_OUTER_BOUND('',#2142,.T.);
#1482=FACE_OUTER_BOUND('',#2143,.T.);
#1483=FACE_OUTER_BOUND('',#2144,.T.);
#1484=FACE_OUTER_BOUND('',#2145,.T.);
#1485=FACE_OUTER_BOUND('',#2146,.T.);
#1486=FACE_OUTER_BOUND('',#2147,.T.);
#1487=FACE_OUTER_BOUND('',#2148,.T.);
#1488=FACE_OUTER_BOUND('',#2149,.T.);
#1489=FACE_OUTER_BOUND('',#2150,.T.);
#1490=FACE_OUTER_BOUND('',#2151,.T.);
#1491=FACE_OUTER_BOUND('',#2152,.T.);
#1492=FACE_OUTER_BOUND('',#2153,.T.);
#1493=FACE_OUTER_BOUND('',#2154,.T.);
#1494=FACE_OUTER_BOUND('',#2155,.T.);
#1495=FACE_OUTER_BOUND('',#2156,.T.);
#1496=FACE_OUTER_BOUND('',#2157,.T.);
#1497=FACE_OUTER_BOUND('',#2158,.T.);
#1498=FACE_OUTER_BOUND('',#2160,.T.);
#1499=FACE_OUTER_BOUND('',#2161,.T.);
#1500=FACE_OUTER_BOUND('',#2163,.T.);
#1501=FACE_OUTER_BOUND('',#2164,.T.);
#1502=FACE_OUTER_BOUND('',#2166,.T.);
#1503=FACE_OUTER_BOUND('',#2167,.T.);
#1504=FACE_OUTER_BOUND('',#2169,.T.);
#1505=FACE_OUTER_BOUND('',#2170,.T.);
#1506=FACE_OUTER_BOUND('',#2172,.T.);
#1507=FACE_OUTER_BOUND('',#2173,.T.);
#1508=FACE_OUTER_BOUND('',#2174,.T.);
#1509=FACE_OUTER_BOUND('',#2175,.T.);
#1510=FACE_OUTER_BOUND('',#2176,.T.);
#1511=FACE_OUTER_BOUND('',#2177,.T.);
#1512=FACE_OUTER_BOUND('',#2178,.T.);
#1513=FACE_OUTER_BOUND('',#2179,.T.);
#1514=FACE_OUTER_BOUND('',#2180,.T.);
#1515=FACE_OUTER_BOUND('',#2181,.T.);
#1516=FACE_OUTER_BOUND('',#2182,.T.);
#1517=FACE_OUTER_BOUND('',#2183,.T.);
#1518=FACE_OUTER_BOUND('',#2184,.T.);
#1519=FACE_OUTER_BOUND('',#2185,.T.);
#1520=FACE_OUTER_BOUND('',#2186,.T.);
#1521=FACE_OUTER_BOUND('',#2188,.T.);
#1522=FACE_OUTER_BOUND('',#2189,.T.);
#1523=FACE_OUTER_BOUND('',#2190,.T.);
#1524=FACE_OUTER_BOUND('',#2191,.T.);
#1525=FACE_OUTER_BOUND('',#2192,.T.);
#1526=FACE_OUTER_BOUND('',#2193,.T.);
#1527=FACE_OUTER_BOUND('',#2194,.T.);
#1528=FACE_OUTER_BOUND('',#2196,.T.);
#1529=FACE_OUTER_BOUND('',#2197,.T.);
#1530=FACE_OUTER_BOUND('',#2198,.T.);
#1531=FACE_OUTER_BOUND('',#2199,.T.);
#1532=FACE_OUTER_BOUND('',#2200,.T.);
#1533=FACE_OUTER_BOUND('',#2201,.T.);
#1534=FACE_OUTER_BOUND('',#2202,.T.);
#1535=FACE_OUTER_BOUND('',#2203,.T.);
#1536=FACE_OUTER_BOUND('',#2204,.T.);
#1537=FACE_OUTER_BOUND('',#2205,.T.);
#1538=FACE_OUTER_BOUND('',#2206,.T.);
#1539=FACE_OUTER_BOUND('',#2207,.T.);
#1540=FACE_OUTER_BOUND('',#2208,.T.);
#1541=FACE_OUTER_BOUND('',#2209,.T.);
#1542=FACE_OUTER_BOUND('',#2210,.T.);
#1543=FACE_OUTER_BOUND('',#2211,.T.);
#1544=FACE_OUTER_BOUND('',#2212,.T.);
#1545=FACE_OUTER_BOUND('',#2213,.T.);
#1546=FACE_OUTER_BOUND('',#2214,.T.);
#1547=FACE_OUTER_BOUND('',#2215,.T.);
#1548=FACE_OUTER_BOUND('',#2216,.T.);
#1549=FACE_OUTER_BOUND('',#2217,.T.);
#1550=FACE_OUTER_BOUND('',#2219,.T.);
#1551=FACE_OUTER_BOUND('',#2221,.T.);
#1552=FACE_OUTER_BOUND('',#2222,.T.);
#1553=FACE_OUTER_BOUND('',#2223,.T.);
#1554=FACE_OUTER_BOUND('',#2224,.T.);
#1555=FACE_OUTER_BOUND('',#2225,.T.);
#1556=FACE_OUTER_BOUND('',#2226,.T.);
#1557=FACE_OUTER_BOUND('',#2227,.T.);
#1558=FACE_OUTER_BOUND('',#2228,.T.);
#1559=FACE_OUTER_BOUND('',#2230,.T.);
#1560=FACE_OUTER_BOUND('',#2232,.T.);
#1561=FACE_OUTER_BOUND('',#2233,.T.);
#1562=FACE_OUTER_BOUND('',#2234,.T.);
#1563=FACE_OUTER_BOUND('',#2236,.T.);
#1564=FACE_OUTER_BOUND('',#2238,.T.);
#1565=FACE_OUTER_BOUND('',#2239,.T.);
#1566=FACE_OUTER_BOUND('',#2240,.T.);
#1567=FACE_OUTER_BOUND('',#2241,.T.);
#1568=FACE_OUTER_BOUND('',#2243,.T.);
#1569=FACE_OUTER_BOUND('',#2245,.T.);
#1570=FACE_OUTER_BOUND('',#2246,.T.);
#1571=FACE_OUTER_BOUND('',#2247,.T.);
#1572=FACE_OUTER_BOUND('',#2248,.T.);
#1573=FACE_OUTER_BOUND('',#2250,.T.);
#1574=FACE_OUTER_BOUND('',#2252,.T.);
#1575=FACE_OUTER_BOUND('',#2254,.T.);
#1576=FACE_OUTER_BOUND('',#2256,.T.);
#1577=FACE_OUTER_BOUND('',#2257,.T.);
#1578=FACE_OUTER_BOUND('',#2258,.T.);
#1579=FACE_OUTER_BOUND('',#2259,.T.);
#1580=FACE_OUTER_BOUND('',#2261,.T.);
#1581=FACE_OUTER_BOUND('',#2262,.T.);
#1582=FACE_OUTER_BOUND('',#2264,.T.);
#1583=FACE_OUTER_BOUND('',#2265,.T.);
#1584=FACE_OUTER_BOUND('',#2266,.T.);
#1585=FACE_OUTER_BOUND('',#2268,.T.);
#1586=FACE_OUTER_BOUND('',#2269,.T.);
#1587=FACE_OUTER_BOUND('',#2270,.T.);
#1588=FACE_OUTER_BOUND('',#2272,.T.);
#1589=FACE_OUTER_BOUND('',#2274,.T.);
#1590=FACE_OUTER_BOUND('',#2275,.T.);
#1591=FACE_OUTER_BOUND('',#2276,.T.);
#1592=FACE_OUTER_BOUND('',#2278,.T.);
#1593=FACE_OUTER_BOUND('',#2280,.T.);
#1594=FACE_OUTER_BOUND('',#2281,.T.);
#1595=FACE_OUTER_BOUND('',#2282,.T.);
#1596=FACE_OUTER_BOUND('',#2283,.T.);
#1597=FACE_OUTER_BOUND('',#2284,.T.);
#1598=FACE_OUTER_BOUND('',#2286,.T.);
#1599=FACE_OUTER_BOUND('',#2287,.T.);
#1600=FACE_OUTER_BOUND('',#2288,.T.);
#1601=FACE_OUTER_BOUND('',#2289,.T.);
#1602=FACE_OUTER_BOUND('',#2290,.T.);
#1603=FACE_OUTER_BOUND('',#2291,.T.);
#1604=FACE_OUTER_BOUND('',#2292,.T.);
#1605=FACE_OUTER_BOUND('',#2293,.T.);
#1606=FACE_OUTER_BOUND('',#2294,.T.);
#1607=FACE_OUTER_BOUND('',#2295,.T.);
#1608=FACE_OUTER_BOUND('',#2296,.T.);
#1609=FACE_OUTER_BOUND('',#2297,.T.);
#1610=FACE_OUTER_BOUND('',#2298,.T.);
#1611=FACE_OUTER_BOUND('',#2299,.T.);
#1612=FACE_OUTER_BOUND('',#2300,.T.);
#1613=FACE_OUTER_BOUND('',#2301,.T.);
#1614=FACE_OUTER_BOUND('',#2302,.T.);
#1615=FACE_OUTER_BOUND('',#2303,.T.);
#1616=FACE_OUTER_BOUND('',#2305,.T.);
#1617=FACE_OUTER_BOUND('',#2307,.T.);
#1618=FACE_OUTER_BOUND('',#2308,.T.);
#1619=FACE_OUTER_BOUND('',#2309,.T.);
#1620=FACE_OUTER_BOUND('',#2311,.T.);
#1621=FACE_OUTER_BOUND('',#2312,.T.);
#1622=FACE_OUTER_BOUND('',#2313,.T.);
#1623=FACE_OUTER_BOUND('',#2314,.T.);
#1624=FACE_OUTER_BOUND('',#2315,.T.);
#1625=FACE_OUTER_BOUND('',#2316,.T.);
#1626=FACE_OUTER_BOUND('',#2318,.T.);
#1627=FACE_OUTER_BOUND('',#2319,.T.);
#1628=FACE_OUTER_BOUND('',#2321,.T.);
#1629=FACE_OUTER_BOUND('',#2322,.T.);
#1630=FACE_OUTER_BOUND('',#2323,.T.);
#1631=FACE_OUTER_BOUND('',#2325,.T.);
#1632=FACE_OUTER_BOUND('',#2326,.T.);
#1633=FACE_OUTER_BOUND('',#2327,.T.);
#1634=FACE_OUTER_BOUND('',#2329,.T.);
#1635=FACE_OUTER_BOUND('',#2331,.T.);
#1636=FACE_OUTER_BOUND('',#2332,.T.);
#1637=FACE_OUTER_BOUND('',#2333,.T.);
#1638=FACE_OUTER_BOUND('',#2335,.T.);
#1639=FACE_OUTER_BOUND('',#2337,.T.);
#1640=FACE_OUTER_BOUND('',#2338,.T.);
#1641=FACE_OUTER_BOUND('',#2339,.T.);
#1642=FACE_OUTER_BOUND('',#2340,.T.);
#1643=FACE_OUTER_BOUND('',#2341,.T.);
#1644=FACE_OUTER_BOUND('',#2342,.T.);
#1645=FACE_OUTER_BOUND('',#2344,.T.);
#1646=FACE_OUTER_BOUND('',#2346,.T.);
#1647=FACE_OUTER_BOUND('',#2347,.T.);
#1648=FACE_OUTER_BOUND('',#2348,.T.);
#1649=FACE_OUTER_BOUND('',#2349,.T.);
#1650=FACE_OUTER_BOUND('',#2350,.T.);
#1651=FACE_OUTER_BOUND('',#2351,.T.);
#1652=FACE_OUTER_BOUND('',#2353,.T.);
#1653=FACE_OUTER_BOUND('',#2355,.T.);
#1654=FACE_OUTER_BOUND('',#2356,.T.);
#1655=FACE_OUTER_BOUND('',#2357,.T.);
#1656=FACE_OUTER_BOUND('',#2358,.T.);
#1657=FACE_OUTER_BOUND('',#2359,.T.);
#1658=FACE_OUTER_BOUND('',#2360,.T.);
#1659=FACE_OUTER_BOUND('',#2361,.T.);
#1660=FACE_OUTER_BOUND('',#2362,.T.);
#1661=FACE_OUTER_BOUND('',#2363,.T.);
#1662=FACE_OUTER_BOUND('',#2364,.T.);
#1663=FACE_OUTER_BOUND('',#2365,.T.);
#1664=FACE_OUTER_BOUND('',#2366,.T.);
#1665=FACE_OUTER_BOUND('',#2367,.T.);
#1666=FACE_OUTER_BOUND('',#2368,.T.);
#1667=FACE_OUTER_BOUND('',#2369,.T.);
#1668=FACE_OUTER_BOUND('',#2370,.T.);
#1669=FACE_OUTER_BOUND('',#2371,.T.);
#1670=FACE_OUTER_BOUND('',#2372,.T.);
#1671=FACE_OUTER_BOUND('',#2373,.T.);
#1672=FACE_OUTER_BOUND('',#2375,.T.);
#1673=FACE_OUTER_BOUND('',#2376,.T.);
#1674=EDGE_LOOP('',(#5534,#5535,#5536,#5537));
#1675=EDGE_LOOP('',(#5538,#5539,#5540,#5541));
#1676=EDGE_LOOP('',(#5542,#5543,#5544,#5545));
#1677=EDGE_LOOP('',(#5546,#5547,#5548,#5549));
#1678=EDGE_LOOP('',(#5550,#5551,#5552,#5553));
#1679=EDGE_LOOP('',(#5554,#5555,#5556,#5557));
#1680=EDGE_LOOP('',(#5558,#5559,#5560,#5561));
#1681=EDGE_LOOP('',(#5562,#5563,#5564,#5565));
#1682=EDGE_LOOP('',(#5566,#5567,#5568,#5569));
#1683=EDGE_LOOP('',(#5570,#5571,#5572,#5573));
#1684=EDGE_LOOP('',(#5574,#5575,#5576,#5577));
#1685=EDGE_LOOP('',(#5578,#5579,#5580,#5581));
#1686=EDGE_LOOP('',(#5582,#5583,#5584,#5585));
#1687=EDGE_LOOP('',(#5586,#5587,#5588,#5589));
#1688=EDGE_LOOP('',(#5590,#5591,#5592,#5593));
#1689=EDGE_LOOP('',(#5594));
#1690=EDGE_LOOP('',(#5595));
#1691=EDGE_LOOP('',(#5596));
#1692=EDGE_LOOP('',(#5597));
#1693=EDGE_LOOP('',(#5598));
#1694=EDGE_LOOP('',(#5599));
#1695=EDGE_LOOP('',(#5600));
#1696=EDGE_LOOP('',(#5601));
#1697=EDGE_LOOP('',(#5602));
#1698=EDGE_LOOP('',(#5603));
#1699=EDGE_LOOP('',(#5604,#5605,#5606,#5607));
#1700=EDGE_LOOP('',(#5608));
#1701=EDGE_LOOP('',(#5609));
#1702=EDGE_LOOP('',(#5610));
#1703=EDGE_LOOP('',(#5611));
#1704=EDGE_LOOP('',(#5612));
#1705=EDGE_LOOP('',(#5613));
#1706=EDGE_LOOP('',(#5614));
#1707=EDGE_LOOP('',(#5615));
#1708=EDGE_LOOP('',(#5616));
#1709=EDGE_LOOP('',(#5617));
#1710=EDGE_LOOP('',(#5618,#5619,#5620,#5621));
#1711=EDGE_LOOP('',(#5622,#5623,#5624,#5625));
#1712=EDGE_LOOP('',(#5626,#5627,#5628,#5629));
#1713=EDGE_LOOP('',(#5630,#5631,#5632,#5633));
#1714=EDGE_LOOP('',(#5634,#5635,#5636,#5637));
#1715=EDGE_LOOP('',(#5638,#5639,#5640,#5641));
#1716=EDGE_LOOP('',(#5642,#5643,#5644,#5645));
#1717=EDGE_LOOP('',(#5646,#5647,#5648,#5649));
#1718=EDGE_LOOP('',(#5650,#5651,#5652,#5653));
#1719=EDGE_LOOP('',(#5654,#5655,#5656,#5657));
#1720=EDGE_LOOP('',(#5658,#5659,#5660,#5661));
#1721=EDGE_LOOP('',(#5662,#5663,#5664,#5665));
#1722=EDGE_LOOP('',(#5666,#5667,#5668,#5669));
#1723=EDGE_LOOP('',(#5670,#5671,#5672,#5673));
#1724=EDGE_LOOP('',(#5674,#5675,#5676,#5677));
#1725=EDGE_LOOP('',(#5678,#5679,#5680,#5681));
#1726=EDGE_LOOP('',(#5682,#5683,#5684,#5685));
#1727=EDGE_LOOP('',(#5686,#5687,#5688,#5689));
#1728=EDGE_LOOP('',(#5690,#5691,#5692,#5693));
#1729=EDGE_LOOP('',(#5694,#5695,#5696,#5697));
#1730=EDGE_LOOP('',(#5698,#5699,#5700,#5701));
#1731=EDGE_LOOP('',(#5702,#5703,#5704,#5705));
#1732=EDGE_LOOP('',(#5706,#5707,#5708,#5709));
#1733=EDGE_LOOP('',(#5710));
#1734=EDGE_LOOP('',(#5711));
#1735=EDGE_LOOP('',(#5712));
#1736=EDGE_LOOP('',(#5713));
#1737=EDGE_LOOP('',(#5714,#5715,#5716,#5717));
#1738=EDGE_LOOP('',(#5718,#5719,#5720,#5721));
#1739=EDGE_LOOP('',(#5722,#5723,#5724,#5725));
#1740=EDGE_LOOP('',(#5726,#5727,#5728,#5729));
#1741=EDGE_LOOP('',(#5730,#5731,#5732,#5733));
#1742=EDGE_LOOP('',(#5734,#5735,#5736,#5737));
#1743=EDGE_LOOP('',(#5738,#5739,#5740,#5741));
#1744=EDGE_LOOP('',(#5742,#5743,#5744,#5745));
#1745=EDGE_LOOP('',(#5746,#5747,#5748,#5749));
#1746=EDGE_LOOP('',(#5750,#5751,#5752,#5753));
#1747=EDGE_LOOP('',(#5754,#5755,#5756,#5757));
#1748=EDGE_LOOP('',(#5758,#5759,#5760,#5761));
#1749=EDGE_LOOP('',(#5762,#5763,#5764,#5765));
#1750=EDGE_LOOP('',(#5766,#5767,#5768,#5769));
#1751=EDGE_LOOP('',(#5770,#5771,#5772,#5773));
#1752=EDGE_LOOP('',(#5774,#5775,#5776,#5777));
#1753=EDGE_LOOP('',(#5778,#5779,#5780,#5781));
#1754=EDGE_LOOP('',(#5782,#5783,#5784,#5785));
#1755=EDGE_LOOP('',(#5786,#5787,#5788,#5789));
#1756=EDGE_LOOP('',(#5790,#5791,#5792,#5793));
#1757=EDGE_LOOP('',(#5794,#5795,#5796,#5797));
#1758=EDGE_LOOP('',(#5798,#5799,#5800,#5801));
#1759=EDGE_LOOP('',(#5802,#5803,#5804,#5805));
#1760=EDGE_LOOP('',(#5806));
#1761=EDGE_LOOP('',(#5807));
#1762=EDGE_LOOP('',(#5808));
#1763=EDGE_LOOP('',(#5809));
#1764=EDGE_LOOP('',(#5810,#5811,#5812,#5813));
#1765=EDGE_LOOP('',(#5814,#5815,#5816,#5817));
#1766=EDGE_LOOP('',(#5818,#5819,#5820,#5821));
#1767=EDGE_LOOP('',(#5822,#5823,#5824,#5825));
#1768=EDGE_LOOP('',(#5826,#5827,#5828,#5829));
#1769=EDGE_LOOP('',(#5830,#5831,#5832,#5833));
#1770=EDGE_LOOP('',(#5834,#5835,#5836,#5837));
#1771=EDGE_LOOP('',(#5838,#5839,#5840,#5841));
#1772=EDGE_LOOP('',(#5842));
#1773=EDGE_LOOP('',(#5843,#5844,#5845,#5846));
#1774=EDGE_LOOP('',(#5847));
#1775=EDGE_LOOP('',(#5848,#5849,#5850,#5851));
#1776=EDGE_LOOP('',(#5852,#5853,#5854,#5855));
#1777=EDGE_LOOP('',(#5856,#5857,#5858,#5859,#5860,#5861,#5862,#5863));
#1778=EDGE_LOOP('',(#5864));
#1779=EDGE_LOOP('',(#5865));
#1780=EDGE_LOOP('',(#5866));
#1781=EDGE_LOOP('',(#5867));
#1782=EDGE_LOOP('',(#5868));
#1783=EDGE_LOOP('',(#5869,#5870,#5871,#5872));
#1784=EDGE_LOOP('',(#5873,#5874,#5875,#5876,#5877,#5878,#5879,#5880));
#1785=EDGE_LOOP('',(#5881));
#1786=EDGE_LOOP('',(#5882));
#1787=EDGE_LOOP('',(#5883));
#1788=EDGE_LOOP('',(#5884));
#1789=EDGE_LOOP('',(#5885));
#1790=EDGE_LOOP('',(#5886,#5887,#5888,#5889));
#1791=EDGE_LOOP('',(#5890,#5891,#5892,#5893));
#1792=EDGE_LOOP('',(#5894,#5895,#5896,#5897));
#1793=EDGE_LOOP('',(#5898));
#1794=EDGE_LOOP('',(#5899));
#1795=EDGE_LOOP('',(#5900,#5901,#5902,#5903));
#1796=EDGE_LOOP('',(#5904,#5905,#5906,#5907));
#1797=EDGE_LOOP('',(#5908,#5909,#5910,#5911));
#1798=EDGE_LOOP('',(#5912,#5913,#5914,#5915));
#1799=EDGE_LOOP('',(#5916,#5917,#5918,#5919));
#1800=EDGE_LOOP('',(#5920));
#1801=EDGE_LOOP('',(#5921));
#1802=EDGE_LOOP('',(#5922,#5923,#5924,#5925));
#1803=EDGE_LOOP('',(#5926,#5927,#5928,#5929));
#1804=EDGE_LOOP('',(#5930));
#1805=EDGE_LOOP('',(#5931));
#1806=EDGE_LOOP('',(#5932));
#1807=EDGE_LOOP('',(#5933));
#1808=EDGE_LOOP('',(#5934));
#1809=EDGE_LOOP('',(#5935));
#1810=EDGE_LOOP('',(#5936));
#1811=EDGE_LOOP('',(#5937));
#1812=EDGE_LOOP('',(#5938));
#1813=EDGE_LOOP('',(#5939));
#1814=EDGE_LOOP('',(#5940));
#1815=EDGE_LOOP('',(#5941));
#1816=EDGE_LOOP('',(#5942,#5943,#5944,#5945));
#1817=EDGE_LOOP('',(#5946,#5947,#5948,#5949));
#1818=EDGE_LOOP('',(#5950,#5951,#5952,#5953));
#1819=EDGE_LOOP('',(#5954,#5955,#5956,#5957));
#1820=EDGE_LOOP('',(#5958,#5959,#5960,#5961));
#1821=EDGE_LOOP('',(#5962));
#1822=EDGE_LOOP('',(#5963));
#1823=EDGE_LOOP('',(#5964,#5965,#5966,#5967));
#1824=EDGE_LOOP('',(#5968,#5969,#5970,#5971));
#1825=EDGE_LOOP('',(#5972));
#1826=EDGE_LOOP('',(#5973));
#1827=EDGE_LOOP('',(#5974));
#1828=EDGE_LOOP('',(#5975));
#1829=EDGE_LOOP('',(#5976));
#1830=EDGE_LOOP('',(#5977));
#1831=EDGE_LOOP('',(#5978));
#1832=EDGE_LOOP('',(#5979));
#1833=EDGE_LOOP('',(#5980));
#1834=EDGE_LOOP('',(#5981));
#1835=EDGE_LOOP('',(#5982));
#1836=EDGE_LOOP('',(#5983));
#1837=EDGE_LOOP('',(#5984,#5985,#5986,#5987));
#1838=EDGE_LOOP('',(#5988,#5989,#5990,#5991));
#1839=EDGE_LOOP('',(#5992,#5993,#5994,#5995));
#1840=EDGE_LOOP('',(#5996,#5997,#5998,#5999));
#1841=EDGE_LOOP('',(#6000,#6001,#6002,#6003));
#1842=EDGE_LOOP('',(#6004,#6005,#6006,#6007));
#1843=EDGE_LOOP('',(#6008,#6009,#6010,#6011));
#1844=EDGE_LOOP('',(#6012,#6013,#6014,#6015));
#1845=EDGE_LOOP('',(#6016));
#1846=EDGE_LOOP('',(#6017,#6018,#6019,#6020));
#1847=EDGE_LOOP('',(#6021));
#1848=EDGE_LOOP('',(#6022,#6023,#6024,#6025));
#1849=EDGE_LOOP('',(#6026,#6027,#6028,#6029));
#1850=EDGE_LOOP('',(#6030,#6031,#6032,#6033,#6034,#6035,#6036,#6037));
#1851=EDGE_LOOP('',(#6038));
#1852=EDGE_LOOP('',(#6039));
#1853=EDGE_LOOP('',(#6040));
#1854=EDGE_LOOP('',(#6041));
#1855=EDGE_LOOP('',(#6042));
#1856=EDGE_LOOP('',(#6043,#6044,#6045,#6046));
#1857=EDGE_LOOP('',(#6047,#6048,#6049,#6050,#6051,#6052,#6053,#6054));
#1858=EDGE_LOOP('',(#6055));
#1859=EDGE_LOOP('',(#6056));
#1860=EDGE_LOOP('',(#6057));
#1861=EDGE_LOOP('',(#6058));
#1862=EDGE_LOOP('',(#6059));
#1863=EDGE_LOOP('',(#6060,#6061,#6062,#6063));
#1864=EDGE_LOOP('',(#6064,#6065,#6066,#6067));
#1865=EDGE_LOOP('',(#6068,#6069,#6070,#6071));
#1866=EDGE_LOOP('',(#6072));
#1867=EDGE_LOOP('',(#6073));
#1868=EDGE_LOOP('',(#6074,#6075,#6076,#6077));
#1869=EDGE_LOOP('',(#6078,#6079,#6080,#6081));
#1870=EDGE_LOOP('',(#6082,#6083,#6084,#6085));
#1871=EDGE_LOOP('',(#6086,#6087,#6088,#6089));
#1872=EDGE_LOOP('',(#6090,#6091,#6092,#6093));
#1873=EDGE_LOOP('',(#6094));
#1874=EDGE_LOOP('',(#6095));
#1875=EDGE_LOOP('',(#6096,#6097,#6098,#6099));
#1876=EDGE_LOOP('',(#6100,#6101,#6102,#6103));
#1877=EDGE_LOOP('',(#6104));
#1878=EDGE_LOOP('',(#6105));
#1879=EDGE_LOOP('',(#6106));
#1880=EDGE_LOOP('',(#6107));
#1881=EDGE_LOOP('',(#6108));
#1882=EDGE_LOOP('',(#6109));
#1883=EDGE_LOOP('',(#6110));
#1884=EDGE_LOOP('',(#6111));
#1885=EDGE_LOOP('',(#6112));
#1886=EDGE_LOOP('',(#6113));
#1887=EDGE_LOOP('',(#6114));
#1888=EDGE_LOOP('',(#6115));
#1889=EDGE_LOOP('',(#6116,#6117,#6118,#6119));
#1890=EDGE_LOOP('',(#6120,#6121,#6122,#6123));
#1891=EDGE_LOOP('',(#6124,#6125,#6126,#6127));
#1892=EDGE_LOOP('',(#6128,#6129,#6130,#6131));
#1893=EDGE_LOOP('',(#6132,#6133,#6134,#6135));
#1894=EDGE_LOOP('',(#6136));
#1895=EDGE_LOOP('',(#6137));
#1896=EDGE_LOOP('',(#6138,#6139,#6140,#6141));
#1897=EDGE_LOOP('',(#6142,#6143,#6144,#6145));
#1898=EDGE_LOOP('',(#6146));
#1899=EDGE_LOOP('',(#6147));
#1900=EDGE_LOOP('',(#6148));
#1901=EDGE_LOOP('',(#6149));
#1902=EDGE_LOOP('',(#6150));
#1903=EDGE_LOOP('',(#6151));
#1904=EDGE_LOOP('',(#6152));
#1905=EDGE_LOOP('',(#6153));
#1906=EDGE_LOOP('',(#6154));
#1907=EDGE_LOOP('',(#6155));
#1908=EDGE_LOOP('',(#6156));
#1909=EDGE_LOOP('',(#6157));
#1910=EDGE_LOOP('',(#6158,#6159,#6160,#6161));
#1911=EDGE_LOOP('',(#6162,#6163,#6164,#6165));
#1912=EDGE_LOOP('',(#6166,#6167,#6168,#6169));
#1913=EDGE_LOOP('',(#6170,#6171,#6172,#6173));
#1914=EDGE_LOOP('',(#6174,#6175,#6176,#6177));
#1915=EDGE_LOOP('',(#6178,#6179,#6180,#6181));
#1916=EDGE_LOOP('',(#6182,#6183,#6184,#6185));
#1917=EDGE_LOOP('',(#6186,#6187,#6188,#6189));
#1918=EDGE_LOOP('',(#6190));
#1919=EDGE_LOOP('',(#6191,#6192,#6193,#6194));
#1920=EDGE_LOOP('',(#6195));
#1921=EDGE_LOOP('',(#6196,#6197,#6198,#6199));
#1922=EDGE_LOOP('',(#6200,#6201,#6202,#6203));
#1923=EDGE_LOOP('',(#6204,#6205,#6206,#6207,#6208,#6209,#6210,#6211));
#1924=EDGE_LOOP('',(#6212,#6213,#6214,#6215));
#1925=EDGE_LOOP('',(#6216));
#1926=EDGE_LOOP('',(#6217));
#1927=EDGE_LOOP('',(#6218));
#1928=EDGE_LOOP('',(#6219));
#1929=EDGE_LOOP('',(#6220));
#1930=EDGE_LOOP('',(#6221,#6222,#6223,#6224,#6225,#6226,#6227,#6228));
#1931=EDGE_LOOP('',(#6229,#6230,#6231,#6232));
#1932=EDGE_LOOP('',(#6233));
#1933=EDGE_LOOP('',(#6234));
#1934=EDGE_LOOP('',(#6235));
#1935=EDGE_LOOP('',(#6236));
#1936=EDGE_LOOP('',(#6237));
#1937=EDGE_LOOP('',(#6238,#6239,#6240,#6241));
#1938=EDGE_LOOP('',(#6242,#6243,#6244,#6245));
#1939=EDGE_LOOP('',(#6246));
#1940=EDGE_LOOP('',(#6247));
#1941=EDGE_LOOP('',(#6248,#6249,#6250,#6251));
#1942=EDGE_LOOP('',(#6252,#6253,#6254,#6255));
#1943=EDGE_LOOP('',(#6256,#6257,#6258,#6259));
#1944=EDGE_LOOP('',(#6260,#6261,#6262,#6263));
#1945=EDGE_LOOP('',(#6264,#6265,#6266,#6267));
#1946=EDGE_LOOP('',(#6268));
#1947=EDGE_LOOP('',(#6269));
#1948=EDGE_LOOP('',(#6270,#6271,#6272,#6273));
#1949=EDGE_LOOP('',(#6274,#6275,#6276,#6277));
#1950=EDGE_LOOP('',(#6278));
#1951=EDGE_LOOP('',(#6279));
#1952=EDGE_LOOP('',(#6280));
#1953=EDGE_LOOP('',(#6281));
#1954=EDGE_LOOP('',(#6282));
#1955=EDGE_LOOP('',(#6283));
#1956=EDGE_LOOP('',(#6284));
#1957=EDGE_LOOP('',(#6285));
#1958=EDGE_LOOP('',(#6286));
#1959=EDGE_LOOP('',(#6287));
#1960=EDGE_LOOP('',(#6288));
#1961=EDGE_LOOP('',(#6289));
#1962=EDGE_LOOP('',(#6290,#6291,#6292,#6293));
#1963=EDGE_LOOP('',(#6294,#6295,#6296,#6297));
#1964=EDGE_LOOP('',(#6298,#6299,#6300,#6301));
#1965=EDGE_LOOP('',(#6302,#6303,#6304,#6305));
#1966=EDGE_LOOP('',(#6306,#6307,#6308,#6309));
#1967=EDGE_LOOP('',(#6310));
#1968=EDGE_LOOP('',(#6311));
#1969=EDGE_LOOP('',(#6312,#6313,#6314,#6315));
#1970=EDGE_LOOP('',(#6316,#6317,#6318,#6319));
#1971=EDGE_LOOP('',(#6320));
#1972=EDGE_LOOP('',(#6321));
#1973=EDGE_LOOP('',(#6322));
#1974=EDGE_LOOP('',(#6323));
#1975=EDGE_LOOP('',(#6324));
#1976=EDGE_LOOP('',(#6325));
#1977=EDGE_LOOP('',(#6326));
#1978=EDGE_LOOP('',(#6327));
#1979=EDGE_LOOP('',(#6328));
#1980=EDGE_LOOP('',(#6329));
#1981=EDGE_LOOP('',(#6330));
#1982=EDGE_LOOP('',(#6331));
#1983=EDGE_LOOP('',(#6332,#6333,#6334,#6335));
#1984=EDGE_LOOP('',(#6336,#6337,#6338,#6339));
#1985=EDGE_LOOP('',(#6340,#6341,#6342,#6343));
#1986=EDGE_LOOP('',(#6344,#6345,#6346,#6347));
#1987=EDGE_LOOP('',(#6348,#6349,#6350,#6351));
#1988=EDGE_LOOP('',(#6352,#6353,#6354,#6355));
#1989=EDGE_LOOP('',(#6356,#6357,#6358,#6359));
#1990=EDGE_LOOP('',(#6360,#6361,#6362,#6363));
#1991=EDGE_LOOP('',(#6364));
#1992=EDGE_LOOP('',(#6365,#6366,#6367,#6368));
#1993=EDGE_LOOP('',(#6369));
#1994=EDGE_LOOP('',(#6370,#6371,#6372,#6373));
#1995=EDGE_LOOP('',(#6374,#6375,#6376,#6377));
#1996=EDGE_LOOP('',(#6378,#6379,#6380,#6381,#6382,#6383,#6384,#6385));
#1997=EDGE_LOOP('',(#6386,#6387,#6388,#6389));
#1998=EDGE_LOOP('',(#6390));
#1999=EDGE_LOOP('',(#6391));
#2000=EDGE_LOOP('',(#6392));
#2001=EDGE_LOOP('',(#6393));
#2002=EDGE_LOOP('',(#6394));
#2003=EDGE_LOOP('',(#6395,#6396,#6397,#6398,#6399,#6400,#6401,#6402));
#2004=EDGE_LOOP('',(#6403,#6404,#6405,#6406));
#2005=EDGE_LOOP('',(#6407));
#2006=EDGE_LOOP('',(#6408));
#2007=EDGE_LOOP('',(#6409));
#2008=EDGE_LOOP('',(#6410));
#2009=EDGE_LOOP('',(#6411));
#2010=EDGE_LOOP('',(#6412,#6413,#6414,#6415));
#2011=EDGE_LOOP('',(#6416,#6417,#6418,#6419));
#2012=EDGE_LOOP('',(#6420));
#2013=EDGE_LOOP('',(#6421));
#2014=EDGE_LOOP('',(#6422,#6423,#6424,#6425));
#2015=EDGE_LOOP('',(#6426,#6427,#6428,#6429));
#2016=EDGE_LOOP('',(#6430,#6431,#6432,#6433));
#2017=EDGE_LOOP('',(#6434,#6435,#6436,#6437));
#2018=EDGE_LOOP('',(#6438,#6439,#6440,#6441));
#2019=EDGE_LOOP('',(#6442));
#2020=EDGE_LOOP('',(#6443));
#2021=EDGE_LOOP('',(#6444,#6445,#6446,#6447));
#2022=EDGE_LOOP('',(#6448,#6449,#6450,#6451));
#2023=EDGE_LOOP('',(#6452));
#2024=EDGE_LOOP('',(#6453));
#2025=EDGE_LOOP('',(#6454));
#2026=EDGE_LOOP('',(#6455));
#2027=EDGE_LOOP('',(#6456));
#2028=EDGE_LOOP('',(#6457));
#2029=EDGE_LOOP('',(#6458));
#2030=EDGE_LOOP('',(#6459));
#2031=EDGE_LOOP('',(#6460));
#2032=EDGE_LOOP('',(#6461));
#2033=EDGE_LOOP('',(#6462));
#2034=EDGE_LOOP('',(#6463));
#2035=EDGE_LOOP('',(#6464,#6465,#6466,#6467));
#2036=EDGE_LOOP('',(#6468,#6469,#6470,#6471));
#2037=EDGE_LOOP('',(#6472,#6473,#6474,#6475));
#2038=EDGE_LOOP('',(#6476,#6477,#6478,#6479));
#2039=EDGE_LOOP('',(#6480,#6481,#6482,#6483));
#2040=EDGE_LOOP('',(#6484));
#2041=EDGE_LOOP('',(#6485));
#2042=EDGE_LOOP('',(#6486,#6487,#6488,#6489));
#2043=EDGE_LOOP('',(#6490,#6491,#6492,#6493));
#2044=EDGE_LOOP('',(#6494));
#2045=EDGE_LOOP('',(#6495));
#2046=EDGE_LOOP('',(#6496));
#2047=EDGE_LOOP('',(#6497));
#2048=EDGE_LOOP('',(#6498));
#2049=EDGE_LOOP('',(#6499));
#2050=EDGE_LOOP('',(#6500));
#2051=EDGE_LOOP('',(#6501));
#2052=EDGE_LOOP('',(#6502));
#2053=EDGE_LOOP('',(#6503));
#2054=EDGE_LOOP('',(#6504));
#2055=EDGE_LOOP('',(#6505));
#2056=EDGE_LOOP('',(#6506,#6507,#6508,#6509));
#2057=EDGE_LOOP('',(#6510,#6511,#6512,#6513));
#2058=EDGE_LOOP('',(#6514,#6515,#6516,#6517));
#2059=EDGE_LOOP('',(#6518));
#2060=EDGE_LOOP('',(#6519));
#2061=EDGE_LOOP('',(#6520,#6521,#6522,#6523));
#2062=EDGE_LOOP('',(#6524,#6525,#6526,#6527));
#2063=EDGE_LOOP('',(#6528));
#2064=EDGE_LOOP('',(#6529));
#2065=EDGE_LOOP('',(#6530,#6531,#6532,#6533));
#2066=EDGE_LOOP('',(#6534,#6535,#6536,#6537));
#2067=EDGE_LOOP('',(#6538));
#2068=EDGE_LOOP('',(#6539));
#2069=EDGE_LOOP('',(#6540,#6541,#6542,#6543));
#2070=EDGE_LOOP('',(#6544,#6545,#6546,#6547));
#2071=EDGE_LOOP('',(#6548));
#2072=EDGE_LOOP('',(#6549));
#2073=EDGE_LOOP('',(#6550,#6551,#6552,#6553));
#2074=EDGE_LOOP('',(#6554,#6555,#6556,#6557));
#2075=EDGE_LOOP('',(#6558));
#2076=EDGE_LOOP('',(#6559));
#2077=EDGE_LOOP('',(#6560,#6561,#6562,#6563));
#2078=EDGE_LOOP('',(#6564));
#2079=EDGE_LOOP('',(#6565));
#2080=EDGE_LOOP('',(#6566,#6567,#6568,#6569));
#2081=EDGE_LOOP('',(#6570));
#2082=EDGE_LOOP('',(#6571));
#2083=EDGE_LOOP('',(#6572,#6573,#6574,#6575));
#2084=EDGE_LOOP('',(#6576));
#2085=EDGE_LOOP('',(#6577));
#2086=EDGE_LOOP('',(#6578,#6579,#6580,#6581));
#2087=EDGE_LOOP('',(#6582));
#2088=EDGE_LOOP('',(#6583));
#2089=EDGE_LOOP('',(#6584,#6585,#6586,#6587));
#2090=EDGE_LOOP('',(#6588));
#2091=EDGE_LOOP('',(#6589));
#2092=EDGE_LOOP('',(#6590,#6591,#6592,#6593));
#2093=EDGE_LOOP('',(#6594));
#2094=EDGE_LOOP('',(#6595));
#2095=EDGE_LOOP('',(#6596,#6597,#6598,#6599));
#2096=EDGE_LOOP('',(#6600));
#2097=EDGE_LOOP('',(#6601));
#2098=EDGE_LOOP('',(#6602));
#2099=EDGE_LOOP('',(#6603,#6604,#6605,#6606));
#2100=EDGE_LOOP('',(#6607,#6608,#6609,#6610));
#2101=EDGE_LOOP('',(#6611,#6612,#6613,#6614));
#2102=EDGE_LOOP('',(#6615));
#2103=EDGE_LOOP('',(#6616));
#2104=EDGE_LOOP('',(#6617,#6618,#6619,#6620));
#2105=EDGE_LOOP('',(#6621,#6622,#6623,#6624));
#2106=EDGE_LOOP('',(#6625,#6626,#6627,#6628));
#2107=EDGE_LOOP('',(#6629));
#2108=EDGE_LOOP('',(#6630,#6631,#6632,#6633));
#2109=EDGE_LOOP('',(#6634,#6635,#6636,#6637));
#2110=EDGE_LOOP('',(#6638,#6639,#6640,#6641));
#2111=EDGE_LOOP('',(#6642,#6643,#6644,#6645));
#2112=EDGE_LOOP('',(#6646,#6647,#6648,#6649));
#2113=EDGE_LOOP('',(#6650,#6651,#6652,#6653));
#2114=EDGE_LOOP('',(#6654,#6655,#6656,#6657,#6658,#6659));
#2115=EDGE_LOOP('',(#6660,#6661,#6662,#6663,#6664,#6665));
#2116=EDGE_LOOP('',(#6666,#6667,#6668,#6669,#6670,#6671));
#2117=EDGE_LOOP('',(#6672,#6673,#6674,#6675,#6676));
#2118=EDGE_LOOP('',(#6677,#6678,#6679,#6680));
#2119=EDGE_LOOP('',(#6681,#6682,#6683,#6684));
#2120=EDGE_LOOP('',(#6685));
#2121=EDGE_LOOP('',(#6686));
#2122=EDGE_LOOP('',(#6687,#6688,#6689,#6690,#6691));
#2123=EDGE_LOOP('',(#6692));
#2124=EDGE_LOOP('',(#6693));
#2125=EDGE_LOOP('',(#6694,#6695,#6696,#6697));
#2126=EDGE_LOOP('',(#6698,#6699,#6700,#6701,#6702,#6703));
#2127=EDGE_LOOP('',(#6704,#6705,#6706,#6707,#6708));
#2128=EDGE_LOOP('',(#6709));
#2129=EDGE_LOOP('',(#6710));
#2130=EDGE_LOOP('',(#6711,#6712,#6713,#6714));
#2131=EDGE_LOOP('',(#6715,#6716,#6717,#6718));
#2132=EDGE_LOOP('',(#6719,#6720,#6721,#6722));
#2133=EDGE_LOOP('',(#6723));
#2134=EDGE_LOOP('',(#6724));
#2135=EDGE_LOOP('',(#6725,#6726,#6727,#6728,#6729));
#2136=EDGE_LOOP('',(#6730,#6731));
#2137=EDGE_LOOP('',(#6732,#6733));
#2138=EDGE_LOOP('',(#6734,#6735));
#2139=EDGE_LOOP('',(#6736,#6737));
#2140=EDGE_LOOP('',(#6738,#6739));
#2141=EDGE_LOOP('',(#6740,#6741));
#2142=EDGE_LOOP('',(#6742,#6743));
#2143=EDGE_LOOP('',(#6744,#6745,#6746,#6747));
#2144=EDGE_LOOP('',(#6748,#6749,#6750,#6751,#6752,#6753,#6754,#6755,#6756,
#6757,#6758,#6759,#6760,#6761,#6762,#6763,#6764,#6765));
#2145=EDGE_LOOP('',(#6766,#6767,#6768,#6769));
#2146=EDGE_LOOP('',(#6770,#6771,#6772,#6773));
#2147=EDGE_LOOP('',(#6774,#6775,#6776,#6777));
#2148=EDGE_LOOP('',(#6778,#6779,#6780,#6781));
#2149=EDGE_LOOP('',(#6782,#6783,#6784,#6785,#6786,#6787));
#2150=EDGE_LOOP('',(#6788,#6789,#6790,#6791));
#2151=EDGE_LOOP('',(#6792,#6793,#6794,#6795));
#2152=EDGE_LOOP('',(#6796,#6797,#6798,#6799));
#2153=EDGE_LOOP('',(#6800,#6801,#6802,#6803));
#2154=EDGE_LOOP('',(#6804,#6805,#6806,#6807));
#2155=EDGE_LOOP('',(#6808,#6809,#6810,#6811,#6812,#6813,#6814,#6815,#6816,
#6817,#6818,#6819,#6820,#6821,#6822,#6823,#6824,#6825));
#2156=EDGE_LOOP('',(#6826,#6827,#6828,#6829));
#2157=EDGE_LOOP('',(#6830,#6831,#6832,#6833));
#2158=EDGE_LOOP('',(#6834));
#2159=EDGE_LOOP('',(#6835));
#2160=EDGE_LOOP('',(#6836,#6837,#6838,#6839));
#2161=EDGE_LOOP('',(#6840));
#2162=EDGE_LOOP('',(#6841));
#2163=EDGE_LOOP('',(#6842,#6843,#6844,#6845));
#2164=EDGE_LOOP('',(#6846));
#2165=EDGE_LOOP('',(#6847));
#2166=EDGE_LOOP('',(#6848,#6849,#6850,#6851));
#2167=EDGE_LOOP('',(#6852));
#2168=EDGE_LOOP('',(#6853));
#2169=EDGE_LOOP('',(#6854,#6855,#6856,#6857));
#2170=EDGE_LOOP('',(#6858));
#2171=EDGE_LOOP('',(#6859));
#2172=EDGE_LOOP('',(#6860,#6861,#6862,#6863));
#2173=EDGE_LOOP('',(#6864,#6865,#6866,#6867));
#2174=EDGE_LOOP('',(#6868,#6869,#6870,#6871));
#2175=EDGE_LOOP('',(#6872,#6873,#6874,#6875));
#2176=EDGE_LOOP('',(#6876,#6877,#6878,#6879));
#2177=EDGE_LOOP('',(#6880,#6881,#6882,#6883));
#2178=EDGE_LOOP('',(#6884,#6885,#6886,#6887));
#2179=EDGE_LOOP('',(#6888,#6889,#6890,#6891,#6892,#6893));
#2180=EDGE_LOOP('',(#6894,#6895,#6896,#6897,#6898,#6899));
#2181=EDGE_LOOP('',(#6900));
#2182=EDGE_LOOP('',(#6901));
#2183=EDGE_LOOP('',(#6902,#6903,#6904,#6905));
#2184=EDGE_LOOP('',(#6906,#6907,#6908,#6909));
#2185=EDGE_LOOP('',(#6910,#6911,#6912,#6913));
#2186=EDGE_LOOP('',(#6914));
#2187=EDGE_LOOP('',(#6915));
#2188=EDGE_LOOP('',(#6916,#6917,#6918,#6919));
#2189=EDGE_LOOP('',(#6920,#6921,#6922,#6923));
#2190=EDGE_LOOP('',(#6924));
#2191=EDGE_LOOP('',(#6925,#6926,#6927,#6928));
#2192=EDGE_LOOP('',(#6929,#6930,#6931,#6932));
#2193=EDGE_LOOP('',(#6933,#6934,#6935,#6936));
#2194=EDGE_LOOP('',(#6937));
#2195=EDGE_LOOP('',(#6938));
#2196=EDGE_LOOP('',(#6939,#6940,#6941,#6942));
#2197=EDGE_LOOP('',(#6943,#6944,#6945,#6946));
#2198=EDGE_LOOP('',(#6947,#6948,#6949,#6950));
#2199=EDGE_LOOP('',(#6951));
#2200=EDGE_LOOP('',(#6952,#6953,#6954,#6955));
#2201=EDGE_LOOP('',(#6956,#6957,#6958,#6959));
#2202=EDGE_LOOP('',(#6960,#6961,#6962,#6963));
#2203=EDGE_LOOP('',(#6964,#6965,#6966,#6967));
#2204=EDGE_LOOP('',(#6968,#6969,#6970,#6971));
#2205=EDGE_LOOP('',(#6972,#6973,#6974,#6975));
#2206=EDGE_LOOP('',(#6976,#6977,#6978,#6979,#6980,#6981));
#2207=EDGE_LOOP('',(#6982,#6983,#6984,#6985,#6986,#6987));
#2208=EDGE_LOOP('',(#6988,#6989,#6990,#6991,#6992,#6993,#6994,#6995,#6996));
#2209=EDGE_LOOP('',(#6997,#6998,#6999,#7000,#7001,#7002,#7003,#7004,#7005));
#2210=EDGE_LOOP('',(#7006,#7007,#7008,#7009));
#2211=EDGE_LOOP('',(#7010,#7011,#7012,#7013));
#2212=EDGE_LOOP('',(#7014,#7015,#7016,#7017));
#2213=EDGE_LOOP('',(#7018,#7019,#7020,#7021));
#2214=EDGE_LOOP('',(#7022,#7023,#7024,#7025));
#2215=EDGE_LOOP('',(#7026,#7027,#7028,#7029));
#2216=EDGE_LOOP('',(#7030,#7031,#7032,#7033));
#2217=EDGE_LOOP('',(#7034));
#2218=EDGE_LOOP('',(#7035));
#2219=EDGE_LOOP('',(#7036));
#2220=EDGE_LOOP('',(#7037));
#2221=EDGE_LOOP('',(#7038,#7039,#7040,#7041));
#2222=EDGE_LOOP('',(#7042));
#2223=EDGE_LOOP('',(#7043,#7044,#7045,#7046));
#2224=EDGE_LOOP('',(#7047,#7048,#7049,#7050));
#2225=EDGE_LOOP('',(#7051,#7052,#7053,#7054));
#2226=EDGE_LOOP('',(#7055,#7056,#7057,#7058));
#2227=EDGE_LOOP('',(#7059,#7060,#7061,#7062));
#2228=EDGE_LOOP('',(#7063));
#2229=EDGE_LOOP('',(#7064));
#2230=EDGE_LOOP('',(#7065));
#2231=EDGE_LOOP('',(#7066));
#2232=EDGE_LOOP('',(#7067,#7068,#7069,#7070));
#2233=EDGE_LOOP('',(#7071,#7072,#7073,#7074));
#2234=EDGE_LOOP('',(#7075,#7076,#7077,#7078));
#2235=EDGE_LOOP('',(#7079,#7080,#7081,#7082));
#2236=EDGE_LOOP('',(#7083));
#2237=EDGE_LOOP('',(#7084));
#2238=EDGE_LOOP('',(#7085));
#2239=EDGE_LOOP('',(#7086,#7087,#7088,#7089));
#2240=EDGE_LOOP('',(#7090,#7091,#7092,#7093));
#2241=EDGE_LOOP('',(#7094));
#2242=EDGE_LOOP('',(#7095));
#2243=EDGE_LOOP('',(#7096));
#2244=EDGE_LOOP('',(#7097));
#2245=EDGE_LOOP('',(#7098,#7099));
#2246=EDGE_LOOP('',(#7100,#7101,#7102,#7103,#7104,#7105,#7106,#7107,#7108));
#2247=EDGE_LOOP('',(#7109,#7110,#7111));
#2248=EDGE_LOOP('',(#7112,#7113,#7114,#7115));
#2249=EDGE_LOOP('',(#7116,#7117,#7118,#7119));
#2250=EDGE_LOOP('',(#7120,#7121,#7122,#7123));
#2251=EDGE_LOOP('',(#7124,#7125));
#2252=EDGE_LOOP('',(#7126));
#2253=EDGE_LOOP('',(#7127));
#2254=EDGE_LOOP('',(#7128));
#2255=EDGE_LOOP('',(#7129));
#2256=EDGE_LOOP('',(#7130,#7131,#7132,#7133));
#2257=EDGE_LOOP('',(#7134,#7135,#7136,#7137));
#2258=EDGE_LOOP('',(#7138,#7139,#7140,#7141));
#2259=EDGE_LOOP('',(#7142));
#2260=EDGE_LOOP('',(#7143,#7144,#7145,#7146));
#2261=EDGE_LOOP('',(#7147,#7148,#7149,#7150));
#2262=EDGE_LOOP('',(#7151));
#2263=EDGE_LOOP('',(#7152));
#2264=EDGE_LOOP('',(#7153,#7154,#7155,#7156));
#2265=EDGE_LOOP('',(#7157,#7158,#7159,#7160));
#2266=EDGE_LOOP('',(#7161));
#2267=EDGE_LOOP('',(#7162,#7163,#7164,#7165));
#2268=EDGE_LOOP('',(#7166,#7167,#7168,#7169));
#2269=EDGE_LOOP('',(#7170,#7171,#7172,#7173));
#2270=EDGE_LOOP('',(#7174));
#2271=EDGE_LOOP('',(#7175));
#2272=EDGE_LOOP('',(#7176));
#2273=EDGE_LOOP('',(#7177));
#2274=EDGE_LOOP('',(#7178,#7179,#7180,#7181));
#2275=EDGE_LOOP('',(#7182,#7183,#7184,#7185));
#2276=EDGE_LOOP('',(#7186));
#2277=EDGE_LOOP('',(#7187));
#2278=EDGE_LOOP('',(#7188));
#2279=EDGE_LOOP('',(#7189));
#2280=EDGE_LOOP('',(#7190));
#2281=EDGE_LOOP('',(#7191,#7192,#7193,#7194));
#2282=EDGE_LOOP('',(#7195,#7196,#7197,#7198));
#2283=EDGE_LOOP('',(#7199,#7200,#7201,#7202));
#2284=EDGE_LOOP('',(#7203));
#2285=EDGE_LOOP('',(#7204));
#2286=EDGE_LOOP('',(#7205,#7206,#7207,#7208));
#2287=EDGE_LOOP('',(#7209,#7210,#7211,#7212));
#2288=EDGE_LOOP('',(#7213,#7214,#7215,#7216));
#2289=EDGE_LOOP('',(#7217));
#2290=EDGE_LOOP('',(#7218,#7219,#7220,#7221));
#2291=EDGE_LOOP('',(#7222,#7223,#7224,#7225));
#2292=EDGE_LOOP('',(#7226,#7227,#7228,#7229));
#2293=EDGE_LOOP('',(#7230,#7231,#7232,#7233));
#2294=EDGE_LOOP('',(#7234,#7235,#7236,#7237));
#2295=EDGE_LOOP('',(#7238,#7239,#7240,#7241));
#2296=EDGE_LOOP('',(#7242,#7243,#7244,#7245,#7246,#7247));
#2297=EDGE_LOOP('',(#7248,#7249,#7250,#7251,#7252,#7253));
#2298=EDGE_LOOP('',(#7254,#7255,#7256,#7257));
#2299=EDGE_LOOP('',(#7258,#7259,#7260,#7261));
#2300=EDGE_LOOP('',(#7262,#7263,#7264,#7265));
#2301=EDGE_LOOP('',(#7266,#7267,#7268,#7269));
#2302=EDGE_LOOP('',(#7270,#7271,#7272,#7273));
#2303=EDGE_LOOP('',(#7274));
#2304=EDGE_LOOP('',(#7275));
#2305=EDGE_LOOP('',(#7276));
#2306=EDGE_LOOP('',(#7277));
#2307=EDGE_LOOP('',(#7278,#7279,#7280,#7281));
#2308=EDGE_LOOP('',(#7282,#7283,#7284,#7285));
#2309=EDGE_LOOP('',(#7286,#7287,#7288,#7289));
#2310=EDGE_LOOP('',(#7290,#7291,#7292,#7293));
#2311=EDGE_LOOP('',(#7294));
#2312=EDGE_LOOP('',(#7295));
#2313=EDGE_LOOP('',(#7296,#7297,#7298,#7299));
#2314=EDGE_LOOP('',(#7300,#7301,#7302,#7303));
#2315=EDGE_LOOP('',(#7304,#7305,#7306,#7307));
#2316=EDGE_LOOP('',(#7308));
#2317=EDGE_LOOP('',(#7309,#7310,#7311,#7312));
#2318=EDGE_LOOP('',(#7313,#7314,#7315,#7316));
#2319=EDGE_LOOP('',(#7317));
#2320=EDGE_LOOP('',(#7318));
#2321=EDGE_LOOP('',(#7319,#7320,#7321,#7322));
#2322=EDGE_LOOP('',(#7323,#7324,#7325,#7326));
#2323=EDGE_LOOP('',(#7327));
#2324=EDGE_LOOP('',(#7328,#7329,#7330,#7331));
#2325=EDGE_LOOP('',(#7332,#7333,#7334,#7335));
#2326=EDGE_LOOP('',(#7336,#7337,#7338,#7339));
#2327=EDGE_LOOP('',(#7340));
#2328=EDGE_LOOP('',(#7341));
#2329=EDGE_LOOP('',(#7342));
#2330=EDGE_LOOP('',(#7343));
#2331=EDGE_LOOP('',(#7344,#7345,#7346,#7347));
#2332=EDGE_LOOP('',(#7348,#7349,#7350,#7351));
#2333=EDGE_LOOP('',(#7352));
#2334=EDGE_LOOP('',(#7353));
#2335=EDGE_LOOP('',(#7354));
#2336=EDGE_LOOP('',(#7355));
#2337=EDGE_LOOP('',(#7356,#7357));
#2338=EDGE_LOOP('',(#7358,#7359,#7360,#7361,#7362,#7363,#7364,#7365,#7366,
#7367,#7368));
#2339=EDGE_LOOP('',(#7369,#7370));
#2340=EDGE_LOOP('',(#7371,#7372,#7373,#7374,#7375,#7376,#7377,#7378,#7379,
#7380,#7381,#7382));
#2341=EDGE_LOOP('',(#7383,#7384,#7385,#7386,#7387,#7388,#7389,#7390,#7391));
#2342=EDGE_LOOP('',(#7392));
#2343=EDGE_LOOP('',(#7393));
#2344=EDGE_LOOP('',(#7394));
#2345=EDGE_LOOP('',(#7395));
#2346=EDGE_LOOP('',(#7396,#7397));
#2347=EDGE_LOOP('',(#7398,#7399,#7400,#7401,#7402,#7403,#7404,#7405,#7406,
#7407,#7408));
#2348=EDGE_LOOP('',(#7409,#7410));
#2349=EDGE_LOOP('',(#7411,#7412,#7413,#7414,#7415,#7416,#7417,#7418,#7419,
#7420,#7421,#7422));
#2350=EDGE_LOOP('',(#7423,#7424,#7425,#7426,#7427,#7428,#7429,#7430,#7431));
#2351=EDGE_LOOP('',(#7432));
#2352=EDGE_LOOP('',(#7433));
#2353=EDGE_LOOP('',(#7434));
#2354=EDGE_LOOP('',(#7435));
#2355=EDGE_LOOP('',(#7436,#7437,#7438,#7439,#7440,#7441,#7442,#7443));
#2356=EDGE_LOOP('',(#7444,#7445,#7446,#7447));
#2357=EDGE_LOOP('',(#7448,#7449,#7450,#7451));
#2358=EDGE_LOOP('',(#7452,#7453,#7454,#7455));
#2359=EDGE_LOOP('',(#7456,#7457,#7458,#7459));
#2360=EDGE_LOOP('',(#7460,#7461,#7462,#7463,#7464,#7465,#7466,#7467));
#2361=EDGE_LOOP('',(#7468,#7469,#7470,#7471));
#2362=EDGE_LOOP('',(#7472,#7473,#7474,#7475));
#2363=EDGE_LOOP('',(#7476,#7477,#7478,#7479));
#2364=EDGE_LOOP('',(#7480,#7481,#7482,#7483));
#2365=EDGE_LOOP('',(#7484));
#2366=EDGE_LOOP('',(#7485,#7486,#7487,#7488));
#2367=EDGE_LOOP('',(#7489,#7490,#7491,#7492));
#2368=EDGE_LOOP('',(#7493,#7494,#7495,#7496));
#2369=EDGE_LOOP('',(#7497,#7498,#7499,#7500));
#2370=EDGE_LOOP('',(#7501,#7502,#7503,#7504));
#2371=EDGE_LOOP('',(#7505,#7506,#7507,#7508));
#2372=EDGE_LOOP('',(#7509,#7510,#7511,#7512,#7513,#7514));
#2373=EDGE_LOOP('',(#7515));
#2374=EDGE_LOOP('',(#7516,#7517,#7518,#7519,#7520,#7521));
#2375=EDGE_LOOP('',(#7522,#7523,#7524,#7525));
#2376=EDGE_LOOP('',(#7526,#7527,#7528,#7529));
#2377=LINE('',#12382,#2917);
#2378=LINE('',#12388,#2918);
#2379=LINE('',#12394,#2919);
#2380=LINE('',#12400,#2920);
#2381=LINE('',#12406,#2921);
#2382=LINE('',#12412,#2922);
#2383=LINE('',#12418,#2923);
#2384=LINE('',#12424,#2924);
#2385=LINE('',#12430,#2925);
#2386=LINE('',#12436,#2926);
#2387=LINE('',#12441,#2927);
#2388=LINE('',#12443,#2928);
#2389=LINE('',#12445,#2929);
#2390=LINE('',#12446,#2930);
#2391=LINE('',#12449,#2931);
#2392=LINE('',#12451,#2932);
#2393=LINE('',#12452,#2933);
#2394=LINE('',#12455,#2934);
#2395=LINE('',#12457,#2935);
#2396=LINE('',#12458,#2936);
#2397=LINE('',#12460,#2937);
#2398=LINE('',#12461,#2938);
#2399=LINE('',#12468,#2939);
#2400=LINE('',#12470,#2940);
#2401=LINE('',#12472,#2941);
#2402=LINE('',#12473,#2942);
#2403=LINE('',#12476,#2943);
#2404=LINE('',#12478,#2944);
#2405=LINE('',#12479,#2945);
#2406=LINE('',#12482,#2946);
#2407=LINE('',#12484,#2947);
#2408=LINE('',#12485,#2948);
#2409=LINE('',#12487,#2949);
#2410=LINE('',#12488,#2950);
#2411=LINE('',#12495,#2951);
#2412=LINE('',#12497,#2952);
#2413=LINE('',#12499,#2953);
#2414=LINE('',#12500,#2954);
#2415=LINE('',#12503,#2955);
#2416=LINE('',#12505,#2956);
#2417=LINE('',#12506,#2957);
#2418=LINE('',#12509,#2958);
#2419=LINE('',#12511,#2959);
#2420=LINE('',#12512,#2960);
#2421=LINE('',#12514,#2961);
#2422=LINE('',#12515,#2962);
#2423=LINE('',#12523,#2963);
#2424=LINE('',#12529,#2964);
#2425=LINE('',#12535,#2965);
#2426=LINE('',#12541,#2966);
#2427=LINE('',#12546,#2967);
#2428=LINE('',#12550,#2968);
#2429=LINE('',#12555,#2969);
#2430=LINE('',#12559,#2970);
#2431=LINE('',#12564,#2971);
#2432=LINE('',#12566,#2972);
#2433=LINE('',#12568,#2973);
#2434=LINE('',#12569,#2974);
#2435=LINE('',#12570,#2975);
#2436=LINE('',#12571,#2976);
#2437=LINE('',#12576,#2977);
#2438=LINE('',#12579,#2978);
#2439=LINE('',#12584,#2979);
#2440=LINE('',#12587,#2980);
#2441=LINE('',#12592,#2981);
#2442=LINE('',#12595,#2982);
#2443=LINE('',#12597,#2983);
#2444=LINE('',#12599,#2984);
#2445=LINE('',#12602,#2985);
#2446=LINE('',#12604,#2986);
#2447=LINE('',#12608,#2987);
#2448=LINE('',#12610,#2988);
#2449=LINE('',#12613,#2989);
#2450=LINE('',#12615,#2990);
#2451=LINE('',#12618,#2991);
#2452=LINE('',#12620,#2992);
#2453=LINE('',#12624,#2993);
#2454=LINE('',#12626,#2994);
#2455=LINE('',#12629,#2995);
#2456=LINE('',#12631,#2996);
#2457=LINE('',#12634,#2997);
#2458=LINE('',#12636,#2998);
#2459=LINE('',#12640,#2999);
#2460=LINE('',#12642,#3000);
#2461=LINE('',#12645,#3001);
#2462=LINE('',#12647,#3002);
#2463=LINE('',#12651,#3003);
#2464=LINE('',#12652,#3004);
#2465=LINE('',#12653,#3005);
#2466=LINE('',#12656,#3006);
#2467=LINE('',#12657,#3007);
#2468=LINE('',#12660,#3008);
#2469=LINE('',#12661,#3009);
#2470=LINE('',#12663,#3010);
#2471=LINE('',#12670,#3011);
#2472=LINE('',#12676,#3012);
#2473=LINE('',#12682,#3013);
#2474=LINE('',#12688,#3014);
#2475=LINE('',#12694,#3015);
#2476=LINE('',#12700,#3016);
#2477=LINE('',#12706,#3017);
#2478=LINE('',#12711,#3018);
#2479=LINE('',#12713,#3019);
#2480=LINE('',#12715,#3020);
#2481=LINE('',#12716,#3021);
#2482=LINE('',#12720,#3022);
#2483=LINE('',#12722,#3023);
#2484=LINE('',#12724,#3024);
#2485=LINE('',#12725,#3025);
#2486=LINE('',#12728,#3026);
#2487=LINE('',#12730,#3027);
#2488=LINE('',#12731,#3028);
#2489=LINE('',#12734,#3029);
#2490=LINE('',#12736,#3030);
#2491=LINE('',#12737,#3031);
#2492=LINE('',#12740,#3032);
#2493=LINE('',#12742,#3033);
#2494=LINE('',#12743,#3034);
#2495=LINE('',#12744,#3035);
#2496=LINE('',#12747,#3036);
#2497=LINE('',#12748,#3037);
#2498=LINE('',#12751,#3038);
#2499=LINE('',#12752,#3039);
#2500=LINE('',#12753,#3040);
#2501=LINE('',#12755,#3041);
#2502=LINE('',#12763,#3042);
#2503=LINE('',#12769,#3043);
#2504=LINE('',#12775,#3044);
#2505=LINE('',#12781,#3045);
#2506=LINE('',#12787,#3046);
#2507=LINE('',#12794,#3047);
#2508=LINE('',#12800,#3048);
#2509=LINE('',#12809,#3049);
#2510=LINE('',#12815,#3050);
#2511=LINE('',#12821,#3051);
#2512=LINE('',#12827,#3052);
#2513=LINE('',#12833,#3053);
#2514=LINE('',#12841,#3054);
#2515=LINE('',#12846,#3055);
#2516=LINE('',#12855,#3056);
#2517=LINE('',#12861,#3057);
#2518=LINE('',#12867,#3058);
#2519=LINE('',#12873,#3059);
#2520=LINE('',#12879,#3060);
#2521=LINE('',#12885,#3061);
#2522=LINE('',#12891,#3062);
#2523=LINE('',#12896,#3063);
#2524=LINE('',#12898,#3064);
#2525=LINE('',#12900,#3065);
#2526=LINE('',#12901,#3066);
#2527=LINE('',#12905,#3067);
#2528=LINE('',#12907,#3068);
#2529=LINE('',#12909,#3069);
#2530=LINE('',#12910,#3070);
#2531=LINE('',#12913,#3071);
#2532=LINE('',#12915,#3072);
#2533=LINE('',#12916,#3073);
#2534=LINE('',#12919,#3074);
#2535=LINE('',#12921,#3075);
#2536=LINE('',#12922,#3076);
#2537=LINE('',#12925,#3077);
#2538=LINE('',#12927,#3078);
#2539=LINE('',#12928,#3079);
#2540=LINE('',#12929,#3080);
#2541=LINE('',#12932,#3081);
#2542=LINE('',#12933,#3082);
#2543=LINE('',#12936,#3083);
#2544=LINE('',#12937,#3084);
#2545=LINE('',#12938,#3085);
#2546=LINE('',#12940,#3086);
#2547=LINE('',#12948,#3087);
#2548=LINE('',#12954,#3088);
#2549=LINE('',#12960,#3089);
#2550=LINE('',#12966,#3090);
#2551=LINE('',#12972,#3091);
#2552=LINE('',#12979,#3092);
#2553=LINE('',#12985,#3093);
#2554=LINE('',#12994,#3094);
#2555=LINE('',#13000,#3095);
#2556=LINE('',#13006,#3096);
#2557=LINE('',#13012,#3097);
#2558=LINE('',#13018,#3098);
#2559=LINE('',#13026,#3099);
#2560=LINE('',#13031,#3100);
#2561=LINE('',#13040,#3101);
#2562=LINE('',#13046,#3102);
#2563=LINE('',#13052,#3103);
#2564=LINE('',#13058,#3104);
#2565=LINE('',#13064,#3105);
#2566=LINE('',#13070,#3106);
#2567=LINE('',#13076,#3107);
#2568=LINE('',#13081,#3108);
#2569=LINE('',#13083,#3109);
#2570=LINE('',#13085,#3110);
#2571=LINE('',#13086,#3111);
#2572=LINE('',#13090,#3112);
#2573=LINE('',#13092,#3113);
#2574=LINE('',#13094,#3114);
#2575=LINE('',#13095,#3115);
#2576=LINE('',#13098,#3116);
#2577=LINE('',#13100,#3117);
#2578=LINE('',#13101,#3118);
#2579=LINE('',#13104,#3119);
#2580=LINE('',#13106,#3120);
#2581=LINE('',#13107,#3121);
#2582=LINE('',#13110,#3122);
#2583=LINE('',#13112,#3123);
#2584=LINE('',#13113,#3124);
#2585=LINE('',#13114,#3125);
#2586=LINE('',#13117,#3126);
#2587=LINE('',#13118,#3127);
#2588=LINE('',#13121,#3128);
#2589=LINE('',#13122,#3129);
#2590=LINE('',#13123,#3130);
#2591=LINE('',#13125,#3131);
#2592=LINE('',#13133,#3132);
#2593=LINE('',#13139,#3133);
#2594=LINE('',#13145,#3134);
#2595=LINE('',#13151,#3135);
#2596=LINE('',#13157,#3136);
#2597=LINE('',#13164,#3137);
#2598=LINE('',#13170,#3138);
#2599=LINE('',#13179,#3139);
#2600=LINE('',#13185,#3140);
#2601=LINE('',#13191,#3141);
#2602=LINE('',#13197,#3142);
#2603=LINE('',#13203,#3143);
#2604=LINE('',#13211,#3144);
#2605=LINE('',#13216,#3145);
#2606=LINE('',#13225,#3146);
#2607=LINE('',#13231,#3147);
#2608=LINE('',#13237,#3148);
#2609=LINE('',#13243,#3149);
#2610=LINE('',#13249,#3150);
#2611=LINE('',#13255,#3151);
#2612=LINE('',#13261,#3152);
#2613=LINE('',#13266,#3153);
#2614=LINE('',#13268,#3154);
#2615=LINE('',#13270,#3155);
#2616=LINE('',#13271,#3156);
#2617=LINE('',#13275,#3157);
#2618=LINE('',#13277,#3158);
#2619=LINE('',#13279,#3159);
#2620=LINE('',#13280,#3160);
#2621=LINE('',#13283,#3161);
#2622=LINE('',#13285,#3162);
#2623=LINE('',#13286,#3163);
#2624=LINE('',#13289,#3164);
#2625=LINE('',#13291,#3165);
#2626=LINE('',#13292,#3166);
#2627=LINE('',#13295,#3167);
#2628=LINE('',#13297,#3168);
#2629=LINE('',#13298,#3169);
#2630=LINE('',#13299,#3170);
#2631=LINE('',#13302,#3171);
#2632=LINE('',#13303,#3172);
#2633=LINE('',#13306,#3173);
#2634=LINE('',#13307,#3174);
#2635=LINE('',#13308,#3175);
#2636=LINE('',#13310,#3176);
#2637=LINE('',#13318,#3177);
#2638=LINE('',#13324,#3178);
#2639=LINE('',#13330,#3179);
#2640=LINE('',#13336,#3180);
#2641=LINE('',#13342,#3181);
#2642=LINE('',#13349,#3182);
#2643=LINE('',#13355,#3183);
#2644=LINE('',#13364,#3184);
#2645=LINE('',#13370,#3185);
#2646=LINE('',#13376,#3186);
#2647=LINE('',#13382,#3187);
#2648=LINE('',#13388,#3188);
#2649=LINE('',#13396,#3189);
#2650=LINE('',#13401,#3190);
#2651=LINE('',#13410,#3191);
#2652=LINE('',#13416,#3192);
#2653=LINE('',#13422,#3193);
#2654=LINE('',#13430,#3194);
#2655=LINE('',#13435,#3195);
#2656=LINE('',#13443,#3196);
#2657=LINE('',#13447,#3197);
#2658=LINE('',#13449,#3198);
#2659=LINE('',#13451,#3199);
#2660=LINE('',#13452,#3200);
#2661=LINE('',#13455,#3201);
#2662=LINE('',#13457,#3202);
#2663=LINE('',#13458,#3203);
#2664=LINE('',#13461,#3204);
#2665=LINE('',#13463,#3205);
#2666=LINE('',#13464,#3206);
#2667=LINE('',#13466,#3207);
#2668=LINE('',#13467,#3208);
#2669=LINE('',#13475,#3209);
#2670=LINE('',#13484,#3210);
#2671=LINE('',#14413,#3211);
#2672=LINE('',#14422,#3212);
#2673=LINE('',#15331,#3213);
#2674=LINE('',#15335,#3214);
#2675=LINE('',#15339,#3215);
#2676=LINE('',#15346,#3216);
#2677=LINE('',#15350,#3217);
#2678=LINE('',#15354,#3218);
#2679=LINE('',#15359,#3219);
#2680=LINE('',#15361,#3220);
#2681=LINE('',#15363,#3221);
#2682=LINE('',#15364,#3222);
#2683=LINE('',#15367,#3223);
#2684=LINE('',#15369,#3224);
#2685=LINE('',#15370,#3225);
#2686=LINE('',#15373,#3226);
#2687=LINE('',#15375,#3227);
#2688=LINE('',#15376,#3228);
#2689=LINE('',#15379,#3229);
#2690=LINE('',#15381,#3230);
#2691=LINE('',#15382,#3231);
#2692=LINE('',#15385,#3232);
#2693=LINE('',#15387,#3233);
#2694=LINE('',#15388,#3234);
#2695=LINE('',#15390,#3235);
#2696=LINE('',#15391,#3236);
#2697=LINE('',#15408,#3237);
#2698=LINE('',#15414,#3238);
#2699=LINE('',#15418,#3239);
#2700=LINE('',#15424,#3240);
#2701=LINE('',#15429,#3241);
#2702=LINE('',#15444,#3242);
#2703=LINE('',#15453,#3243);
#2704=LINE('',#15457,#3244);
#2705=LINE('',#15461,#3245);
#2706=LINE('',#15464,#3246);
#2707=LINE('',#15600,#3247);
#2708=LINE('',#15853,#3248);
#2709=LINE('',#15895,#3249);
#2710=LINE('',#15900,#3250);
#2711=LINE('',#15909,#3251);
#2712=LINE('',#15914,#3252);
#2713=LINE('',#15924,#3253);
#2714=LINE('',#15926,#3254);
#2715=LINE('',#15928,#3255);
#2716=LINE('',#15929,#3256);
#2717=LINE('',#15932,#3257);
#2718=LINE('',#15934,#3258);
#2719=LINE('',#15935,#3259);
#2720=LINE('',#15938,#3260);
#2721=LINE('',#15940,#3261);
#2722=LINE('',#15941,#3262);
#2723=LINE('',#15944,#3263);
#2724=LINE('',#15946,#3264);
#2725=LINE('',#15947,#3265);
#2726=LINE('',#15950,#3266);
#2727=LINE('',#15952,#3267);
#2728=LINE('',#15953,#3268);
#2729=LINE('',#15955,#3269);
#2730=LINE('',#15956,#3270);
#2731=LINE('',#15968,#3271);
#2732=LINE('',#15972,#3272);
#2733=LINE('',#15976,#3273);
#2734=LINE('',#15983,#3274);
#2735=LINE('',#15985,#3275);
#2736=LINE('',#15993,#3276);
#2737=LINE('',#15997,#3277);
#2738=LINE('',#16001,#3278);
#2739=LINE('',#16008,#3279);
#2740=LINE('',#16012,#3280);
#2741=LINE('',#16016,#3281);
#2742=LINE('',#16021,#3282);
#2743=LINE('',#16023,#3283);
#2744=LINE('',#16025,#3284);
#2745=LINE('',#16026,#3285);
#2746=LINE('',#16029,#3286);
#2747=LINE('',#16031,#3287);
#2748=LINE('',#16032,#3288);
#2749=LINE('',#16035,#3289);
#2750=LINE('',#16037,#3290);
#2751=LINE('',#16038,#3291);
#2752=LINE('',#16041,#3292);
#2753=LINE('',#16043,#3293);
#2754=LINE('',#16044,#3294);
#2755=LINE('',#16047,#3295);
#2756=LINE('',#16049,#3296);
#2757=LINE('',#16050,#3297);
#2758=LINE('',#16052,#3298);
#2759=LINE('',#16053,#3299);
#2760=LINE('',#16068,#3300);
#2761=LINE('',#16089,#3301);
#2762=LINE('',#16114,#3302);
#2763=LINE('',#16115,#3303);
#2764=LINE('',#16117,#3304);
#2765=LINE('',#16119,#3305);
#2766=LINE('',#16124,#3306);
#2767=LINE('',#16127,#3307);
#2768=LINE('',#16129,#3308);
#2769=LINE('',#16139,#3309);
#2770=LINE('',#16145,#3310);
#2771=LINE('',#16147,#3311);
#2772=LINE('',#16149,#3312);
#2773=LINE('',#16150,#3313);
#2774=LINE('',#16155,#3314);
#2775=LINE('',#16156,#3315);
#2776=LINE('',#16159,#3316);
#2777=LINE('',#16161,#3317);
#2778=LINE('',#16162,#3318);
#2779=LINE('',#16164,#3319);
#2780=LINE('',#16178,#3320);
#2781=LINE('',#16181,#3321);
#2782=LINE('',#16186,#3322);
#2783=LINE('',#16194,#3323);
#2784=LINE('',#16200,#3324);
#2785=LINE('',#16208,#3325);
#2786=LINE('',#16225,#3326);
#2787=LINE('',#16276,#3327);
#2788=LINE('',#16281,#3328);
#2789=LINE('',#16287,#3329);
#2790=LINE('',#16295,#3330);
#2791=LINE('',#16297,#3331);
#2792=LINE('',#16299,#3332);
#2793=LINE('',#16300,#3333);
#2794=LINE('',#16303,#3334);
#2795=LINE('',#16305,#3335);
#2796=LINE('',#16306,#3336);
#2797=LINE('',#16309,#3337);
#2798=LINE('',#16311,#3338);
#2799=LINE('',#16312,#3339);
#2800=LINE('',#16325,#3340);
#2801=LINE('',#16328,#3341);
#2802=LINE('',#16336,#3342);
#2803=LINE('',#16342,#3343);
#2804=LINE('',#16351,#3344);
#2805=LINE('',#16357,#3345);
#2806=LINE('',#16368,#3346);
#2807=LINE('',#16372,#3347);
#2808=LINE('',#16376,#3348);
#2809=LINE('',#16383,#3349);
#2810=LINE('',#16387,#3350);
#2811=LINE('',#16391,#3351);
#2812=LINE('',#16396,#3352);
#2813=LINE('',#16398,#3353);
#2814=LINE('',#16400,#3354);
#2815=LINE('',#16401,#3355);
#2816=LINE('',#16404,#3356);
#2817=LINE('',#16406,#3357);
#2818=LINE('',#16407,#3358);
#2819=LINE('',#16410,#3359);
#2820=LINE('',#16412,#3360);
#2821=LINE('',#16413,#3361);
#2822=LINE('',#16416,#3362);
#2823=LINE('',#16418,#3363);
#2824=LINE('',#16419,#3364);
#2825=LINE('',#16422,#3365);
#2826=LINE('',#16424,#3366);
#2827=LINE('',#16425,#3367);
#2828=LINE('',#16427,#3368);
#2829=LINE('',#16428,#3369);
#2830=LINE('',#16513,#3370);
#2831=LINE('',#16515,#3371);
#2832=LINE('',#16517,#3372);
#2833=LINE('',#16518,#3373);
#2834=LINE('',#16523,#3374);
#2835=LINE('',#16524,#3375);
#2836=LINE('',#16527,#3376);
#2837=LINE('',#16528,#3377);
#2838=LINE('',#16531,#3378);
#2839=LINE('',#16532,#3379);
#2840=LINE('',#16546,#3380);
#2841=LINE('',#16549,#3381);
#2842=LINE('',#16554,#3382);
#2843=LINE('',#16561,#3383);
#2844=LINE('',#16563,#3384);
#2845=LINE('',#16565,#3385);
#2846=LINE('',#16566,#3386);
#2847=LINE('',#16569,#3387);
#2848=LINE('',#16571,#3388);
#2849=LINE('',#16572,#3389);
#2850=LINE('',#16575,#3390);
#2851=LINE('',#16577,#3391);
#2852=LINE('',#16578,#3392);
#2853=LINE('',#16592,#3393);
#2854=LINE('',#16595,#3394);
#2855=LINE('',#16602,#3395);
#2856=LINE('',#16608,#3396);
#2857=LINE('',#16617,#3397);
#2858=LINE('',#16623,#3398);
#2859=LINE('',#16631,#3399);
#2860=LINE('',#16664,#3400);
#2861=LINE('',#16706,#3401);
#2862=LINE('',#16710,#3402);
#2863=LINE('',#16712,#3403);
#2864=LINE('',#16717,#3404);
#2865=LINE('',#16719,#3405);
#2866=LINE('',#16727,#3406);
#2867=LINE('',#16760,#3407);
#2868=LINE('',#16802,#3408);
#2869=LINE('',#16806,#3409);
#2870=LINE('',#16808,#3410);
#2871=LINE('',#16813,#3411);
#2872=LINE('',#16815,#3412);
#2873=LINE('',#16823,#3413);
#2874=LINE('',#16825,#3414);
#2875=LINE('',#16827,#3415);
#2876=LINE('',#16829,#3416);
#2877=LINE('',#16831,#3417);
#2878=LINE('',#16833,#3418);
#2879=LINE('',#16835,#3419);
#2880=LINE('',#16836,#3420);
#2881=LINE('',#16839,#3421);
#2882=LINE('',#16841,#3422);
#2883=LINE('',#16842,#3423);
#2884=LINE('',#16845,#3424);
#2885=LINE('',#16846,#3425);
#2886=LINE('',#16849,#3426);
#2887=LINE('',#16850,#3427);
#2888=LINE('',#16853,#3428);
#2889=LINE('',#16854,#3429);
#2890=LINE('',#16857,#3430);
#2891=LINE('',#16859,#3431);
#2892=LINE('',#16861,#3432);
#2893=LINE('',#16862,#3433);
#2894=LINE('',#16864,#3434);
#2895=LINE('',#16866,#3435);
#2896=LINE('',#16868,#3436);
#2897=LINE('',#16877,#3437);
#2898=LINE('',#16879,#3438);
#2899=LINE('',#16881,#3439);
#2900=LINE('',#16882,#3440);
#2901=LINE('',#16885,#3441);
#2902=LINE('',#16887,#3442);
#2903=LINE('',#16888,#3443);
#2904=LINE('',#16891,#3444);
#2905=LINE('',#16893,#3445);
#2906=LINE('',#16894,#3446);
#2907=LINE('',#16897,#3447);
#2908=LINE('',#16899,#3448);
#2909=LINE('',#16900,#3449);
#2910=LINE('',#16903,#3450);
#2911=LINE('',#16905,#3451);
#2912=LINE('',#16906,#3452);
#2913=LINE('',#16908,#3453);
#2914=LINE('',#16909,#3454);
#2915=LINE('',#16917,#3455);
#2916=LINE('',#16919,#3456);
#2917=VECTOR('',#9783,0.165);
#2918=VECTOR('',#9790,0.165);
#2919=VECTOR('',#9797,0.165);
#2920=VECTOR('',#9804,0.165);
#2921=VECTOR('',#9811,0.165);
#2922=VECTOR('',#9818,0.165);
#2923=VECTOR('',#9825,0.210000000000001);
#2924=VECTOR('',#9832,0.21);
#2925=VECTOR('',#9839,0.21);
#2926=VECTOR('',#9846,0.210000000000001);
#2927=VECTOR('',#9851,1.);
#2928=VECTOR('',#9852,1.);
#2929=VECTOR('',#9853,1.);
#2930=VECTOR('',#9854,1.);
#2931=VECTOR('',#9857,1.);
#2932=VECTOR('',#9858,1.);
#2933=VECTOR('',#9859,1.);
#2934=VECTOR('',#9862,1.);
#2935=VECTOR('',#9863,1.);
#2936=VECTOR('',#9864,1.);
#2937=VECTOR('',#9867,1.);
#2938=VECTOR('',#9868,1.);
#2939=VECTOR('',#9877,1.);
#2940=VECTOR('',#9878,1.);
#2941=VECTOR('',#9879,1.);
#2942=VECTOR('',#9880,1.);
#2943=VECTOR('',#9883,1.);
#2944=VECTOR('',#9884,1.);
#2945=VECTOR('',#9885,1.);
#2946=VECTOR('',#9888,1.);
#2947=VECTOR('',#9889,1.);
#2948=VECTOR('',#9890,1.);
#2949=VECTOR('',#9893,1.);
#2950=VECTOR('',#9894,1.);
#2951=VECTOR('',#9903,1.);
#2952=VECTOR('',#9904,1.);
#2953=VECTOR('',#9905,1.);
#2954=VECTOR('',#9906,1.);
#2955=VECTOR('',#9909,1.);
#2956=VECTOR('',#9910,1.);
#2957=VECTOR('',#9911,1.);
#2958=VECTOR('',#9914,1.);
#2959=VECTOR('',#9915,1.);
#2960=VECTOR('',#9916,1.);
#2961=VECTOR('',#9919,1.);
#2962=VECTOR('',#9920,1.);
#2963=VECTOR('',#9931,0.165);
#2964=VECTOR('',#9938,0.165);
#2965=VECTOR('',#9945,0.165);
#2966=VECTOR('',#9952,0.165);
#2967=VECTOR('',#9957,1.);
#2968=VECTOR('',#9960,1.);
#2969=VECTOR('',#9965,1.);
#2970=VECTOR('',#9968,1.);
#2971=VECTOR('',#9973,1.);
#2972=VECTOR('',#9974,1.);
#2973=VECTOR('',#9975,1.);
#2974=VECTOR('',#9976,1.);
#2975=VECTOR('',#9977,1.);
#2976=VECTOR('',#9978,1.);
#2977=VECTOR('',#9981,1.);
#2978=VECTOR('',#9984,1.);
#2979=VECTOR('',#9987,1.);
#2980=VECTOR('',#9990,1.);
#2981=VECTOR('',#9993,1.);
#2982=VECTOR('',#9996,1.);
#2983=VECTOR('',#9999,1.);
#2984=VECTOR('',#10002,1.);
#2985=VECTOR('',#10005,1.);
#2986=VECTOR('',#10006,1.);
#2987=VECTOR('',#10011,1.);
#2988=VECTOR('',#10012,1.);
#2989=VECTOR('',#10017,1.);
#2990=VECTOR('',#10020,1.);
#2991=VECTOR('',#10023,1.);
#2992=VECTOR('',#10024,1.);
#2993=VECTOR('',#10029,1.);
#2994=VECTOR('',#10030,1.);
#2995=VECTOR('',#10035,1.);
#2996=VECTOR('',#10038,1.);
#2997=VECTOR('',#10041,1.);
#2998=VECTOR('',#10042,1.);
#2999=VECTOR('',#10047,1.);
#3000=VECTOR('',#10048,1.);
#3001=VECTOR('',#10053,1.);
#3002=VECTOR('',#10056,1.);
#3003=VECTOR('',#10059,1.);
#3004=VECTOR('',#10060,1.);
#3005=VECTOR('',#10061,1.);
#3006=VECTOR('',#10064,1.);
#3007=VECTOR('',#10065,1.);
#3008=VECTOR('',#10068,1.);
#3009=VECTOR('',#10069,1.);
#3010=VECTOR('',#10072,1.);
#3011=VECTOR('',#10081,0.165);
#3012=VECTOR('',#10088,0.165);
#3013=VECTOR('',#10095,0.165);
#3014=VECTOR('',#10102,0.165);
#3015=VECTOR('',#10109,1.6);
#3016=VECTOR('',#10116,0.225);
#3017=VECTOR('',#10123,0.225);
#3018=VECTOR('',#10128,1.);
#3019=VECTOR('',#10129,1.);
#3020=VECTOR('',#10130,1.);
#3021=VECTOR('',#10131,1.);
#3022=VECTOR('',#10134,1.);
#3023=VECTOR('',#10135,1.);
#3024=VECTOR('',#10136,1.);
#3025=VECTOR('',#10137,1.);
#3026=VECTOR('',#10140,1.);
#3027=VECTOR('',#10141,1.);
#3028=VECTOR('',#10142,1.);
#3029=VECTOR('',#10145,1.);
#3030=VECTOR('',#10146,1.);
#3031=VECTOR('',#10147,1.);
#3032=VECTOR('',#10150,1.);
#3033=VECTOR('',#10151,1.);
#3034=VECTOR('',#10152,1.);
#3035=VECTOR('',#10153,1.);
#3036=VECTOR('',#10156,1.);
#3037=VECTOR('',#10157,1.);
#3038=VECTOR('',#10160,1.);
#3039=VECTOR('',#10161,1.);
#3040=VECTOR('',#10162,1.);
#3041=VECTOR('',#10165,1.);
#3042=VECTOR('',#10176,0.225);
#3043=VECTOR('',#10183,0.225);
#3044=VECTOR('',#10190,0.225);
#3045=VECTOR('',#10197,0.225);
#3046=VECTOR('',#10204,1.59);
#3047=VECTOR('',#10213,1.2);
#3048=VECTOR('',#10220,2.4);
#3049=VECTOR('',#10233,0.225);
#3050=VECTOR('',#10240,0.225);
#3051=VECTOR('',#10247,0.225);
#3052=VECTOR('',#10254,0.225);
#3053=VECTOR('',#10261,1.59);
#3054=VECTOR('',#10272,1.2);
#3055=VECTOR('',#10277,2.4);
#3056=VECTOR('',#10290,0.165);
#3057=VECTOR('',#10297,0.165);
#3058=VECTOR('',#10304,0.165);
#3059=VECTOR('',#10311,0.165);
#3060=VECTOR('',#10318,1.6);
#3061=VECTOR('',#10325,0.225);
#3062=VECTOR('',#10332,0.225);
#3063=VECTOR('',#10337,1.);
#3064=VECTOR('',#10338,1.);
#3065=VECTOR('',#10339,1.);
#3066=VECTOR('',#10340,1.);
#3067=VECTOR('',#10343,1.);
#3068=VECTOR('',#10344,1.);
#3069=VECTOR('',#10345,1.);
#3070=VECTOR('',#10346,1.);
#3071=VECTOR('',#10349,1.);
#3072=VECTOR('',#10350,1.);
#3073=VECTOR('',#10351,1.);
#3074=VECTOR('',#10354,1.);
#3075=VECTOR('',#10355,1.);
#3076=VECTOR('',#10356,1.);
#3077=VECTOR('',#10359,1.);
#3078=VECTOR('',#10360,1.);
#3079=VECTOR('',#10361,1.);
#3080=VECTOR('',#10362,1.);
#3081=VECTOR('',#10365,1.);
#3082=VECTOR('',#10366,1.);
#3083=VECTOR('',#10369,1.);
#3084=VECTOR('',#10370,1.);
#3085=VECTOR('',#10371,1.);
#3086=VECTOR('',#10374,1.);
#3087=VECTOR('',#10385,0.225);
#3088=VECTOR('',#10392,0.225);
#3089=VECTOR('',#10399,0.225);
#3090=VECTOR('',#10406,0.225);
#3091=VECTOR('',#10413,1.59);
#3092=VECTOR('',#10422,1.2);
#3093=VECTOR('',#10429,2.4);
#3094=VECTOR('',#10442,0.225);
#3095=VECTOR('',#10449,0.225);
#3096=VECTOR('',#10456,0.225);
#3097=VECTOR('',#10463,0.225);
#3098=VECTOR('',#10470,1.59);
#3099=VECTOR('',#10481,1.2);
#3100=VECTOR('',#10486,2.4);
#3101=VECTOR('',#10499,0.165);
#3102=VECTOR('',#10506,0.164999999999999);
#3103=VECTOR('',#10513,0.164999999999999);
#3104=VECTOR('',#10520,0.165);
#3105=VECTOR('',#10527,1.6);
#3106=VECTOR('',#10534,0.225);
#3107=VECTOR('',#10541,0.225);
#3108=VECTOR('',#10546,1.);
#3109=VECTOR('',#10547,1.);
#3110=VECTOR('',#10548,1.);
#3111=VECTOR('',#10549,1.);
#3112=VECTOR('',#10552,1.);
#3113=VECTOR('',#10553,1.);
#3114=VECTOR('',#10554,1.);
#3115=VECTOR('',#10555,1.);
#3116=VECTOR('',#10558,1.);
#3117=VECTOR('',#10559,1.);
#3118=VECTOR('',#10560,1.);
#3119=VECTOR('',#10563,1.);
#3120=VECTOR('',#10564,1.);
#3121=VECTOR('',#10565,1.);
#3122=VECTOR('',#10568,1.);
#3123=VECTOR('',#10569,1.);
#3124=VECTOR('',#10570,1.);
#3125=VECTOR('',#10571,1.);
#3126=VECTOR('',#10574,1.);
#3127=VECTOR('',#10575,1.);
#3128=VECTOR('',#10578,1.);
#3129=VECTOR('',#10579,1.);
#3130=VECTOR('',#10580,1.);
#3131=VECTOR('',#10583,1.);
#3132=VECTOR('',#10594,0.225);
#3133=VECTOR('',#10601,0.225);
#3134=VECTOR('',#10608,0.225);
#3135=VECTOR('',#10615,0.225);
#3136=VECTOR('',#10622,1.59);
#3137=VECTOR('',#10631,1.2);
#3138=VECTOR('',#10638,2.4);
#3139=VECTOR('',#10651,0.225);
#3140=VECTOR('',#10658,0.225);
#3141=VECTOR('',#10665,0.225);
#3142=VECTOR('',#10672,0.225);
#3143=VECTOR('',#10679,1.59);
#3144=VECTOR('',#10690,1.2);
#3145=VECTOR('',#10695,2.4);
#3146=VECTOR('',#10708,0.165);
#3147=VECTOR('',#10715,0.164999999999999);
#3148=VECTOR('',#10722,0.164999999999999);
#3149=VECTOR('',#10729,0.165);
#3150=VECTOR('',#10736,1.6);
#3151=VECTOR('',#10743,0.225);
#3152=VECTOR('',#10750,0.225);
#3153=VECTOR('',#10755,1.);
#3154=VECTOR('',#10756,1.);
#3155=VECTOR('',#10757,1.);
#3156=VECTOR('',#10758,1.);
#3157=VECTOR('',#10761,1.);
#3158=VECTOR('',#10762,1.);
#3159=VECTOR('',#10763,1.);
#3160=VECTOR('',#10764,1.);
#3161=VECTOR('',#10767,1.);
#3162=VECTOR('',#10768,1.);
#3163=VECTOR('',#10769,1.);
#3164=VECTOR('',#10772,1.);
#3165=VECTOR('',#10773,1.);
#3166=VECTOR('',#10774,1.);
#3167=VECTOR('',#10777,1.);
#3168=VECTOR('',#10778,1.);
#3169=VECTOR('',#10779,1.);
#3170=VECTOR('',#10780,1.);
#3171=VECTOR('',#10783,1.);
#3172=VECTOR('',#10784,1.);
#3173=VECTOR('',#10787,1.);
#3174=VECTOR('',#10788,1.);
#3175=VECTOR('',#10789,1.);
#3176=VECTOR('',#10792,1.);
#3177=VECTOR('',#10803,0.225);
#3178=VECTOR('',#10810,0.225);
#3179=VECTOR('',#10817,0.225);
#3180=VECTOR('',#10824,0.225);
#3181=VECTOR('',#10831,1.59);
#3182=VECTOR('',#10840,1.2);
#3183=VECTOR('',#10847,2.4);
#3184=VECTOR('',#10860,0.225);
#3185=VECTOR('',#10867,0.225);
#3186=VECTOR('',#10874,0.225);
#3187=VECTOR('',#10881,0.225);
#3188=VECTOR('',#10888,1.59);
#3189=VECTOR('',#10899,1.2);
#3190=VECTOR('',#10904,2.4);
#3191=VECTOR('',#10917,0.25);
#3192=VECTOR('',#10924,0.25);
#3193=VECTOR('',#10931,0.4);
#3194=VECTOR('',#10942,0.225);
#3195=VECTOR('',#10947,0.4);
#3196=VECTOR('',#10958,0.225);
#3197=VECTOR('',#10961,1.);
#3198=VECTOR('',#10962,1.);
#3199=VECTOR('',#10963,1.);
#3200=VECTOR('',#10964,1.);
#3201=VECTOR('',#10967,1.);
#3202=VECTOR('',#10968,1.);
#3203=VECTOR('',#10969,1.);
#3204=VECTOR('',#10972,1.);
#3205=VECTOR('',#10973,1.);
#3206=VECTOR('',#10974,1.);
#3207=VECTOR('',#10977,1.);
#3208=VECTOR('',#10978,1.);
#3209=VECTOR('',#10989,0.7);
#3210=VECTOR('',#11002,0.7);
#3211=VECTOR('',#11025,0.7);
#3212=VECTOR('',#11038,0.7);
#3213=VECTOR('',#11065,0.4);
#3214=VECTOR('',#11070,0.425);
#3215=VECTOR('',#11075,0.41);
#3216=VECTOR('',#11084,0.26);
#3217=VECTOR('',#11089,0.25);
#3218=VECTOR('',#11094,0.225);
#3219=VECTOR('',#11099,1.);
#3220=VECTOR('',#11100,1.);
#3221=VECTOR('',#11101,1.);
#3222=VECTOR('',#11102,1.);
#3223=VECTOR('',#11105,1.);
#3224=VECTOR('',#11106,1.);
#3225=VECTOR('',#11107,1.);
#3226=VECTOR('',#11110,1.);
#3227=VECTOR('',#11111,1.);
#3228=VECTOR('',#11112,1.);
#3229=VECTOR('',#11115,1.);
#3230=VECTOR('',#11116,1.);
#3231=VECTOR('',#11117,1.);
#3232=VECTOR('',#11120,1.);
#3233=VECTOR('',#11121,1.);
#3234=VECTOR('',#11122,1.);
#3235=VECTOR('',#11125,1.);
#3236=VECTOR('',#11126,1.);
#3237=VECTOR('',#11149,1.070235);
#3238=VECTOR('',#11156,0.6);
#3239=VECTOR('',#11161,0.63);
#3240=VECTOR('',#11170,1.070235);
#3241=VECTOR('',#11177,0.63);
#3242=VECTOR('',#11196,1.129765);
#3243=VECTOR('',#11207,1.57);
#3244=VECTOR('',#11212,1.6);
#3245=VECTOR('',#11217,1.57);
#3246=VECTOR('',#11222,1.129765);
#3247=VECTOR('',#11269,1.123812);
#3248=VECTOR('',#11338,1.076188);
#3249=VECTOR('',#11367,1.119765);
#3250=VECTOR('',#11374,1.085235);
#3251=VECTOR('',#11385,1.119765);
#3252=VECTOR('',#11392,1.085235);
#3253=VECTOR('',#11407,1.);
#3254=VECTOR('',#11408,1.);
#3255=VECTOR('',#11409,1.);
#3256=VECTOR('',#11410,1.);
#3257=VECTOR('',#11413,1.);
#3258=VECTOR('',#11414,1.);
#3259=VECTOR('',#11415,1.);
#3260=VECTOR('',#11418,1.);
#3261=VECTOR('',#11419,1.);
#3262=VECTOR('',#11420,1.);
#3263=VECTOR('',#11423,1.);
#3264=VECTOR('',#11424,1.);
#3265=VECTOR('',#11425,1.);
#3266=VECTOR('',#11428,1.);
#3267=VECTOR('',#11429,1.);
#3268=VECTOR('',#11430,1.);
#3269=VECTOR('',#11433,1.);
#3270=VECTOR('',#11434,1.);
#3271=VECTOR('',#11451,0.325);
#3272=VECTOR('',#11456,0.35);
#3273=VECTOR('',#11461,0.335);
#3274=VECTOR('',#11470,0.21);
#3275=VECTOR('',#11473,0.2);
#3276=VECTOR('',#11484,0.475);
#3277=VECTOR('',#11489,0.5);
#3278=VECTOR('',#11494,0.485);
#3279=VECTOR('',#11503,0.31);
#3280=VECTOR('',#11508,0.3);
#3281=VECTOR('',#11513,0.27);
#3282=VECTOR('',#11518,1.);
#3283=VECTOR('',#11519,1.);
#3284=VECTOR('',#11520,1.);
#3285=VECTOR('',#11521,1.);
#3286=VECTOR('',#11524,1.);
#3287=VECTOR('',#11525,1.);
#3288=VECTOR('',#11526,1.);
#3289=VECTOR('',#11529,1.);
#3290=VECTOR('',#11530,1.);
#3291=VECTOR('',#11531,1.);
#3292=VECTOR('',#11534,1.);
#3293=VECTOR('',#11535,1.);
#3294=VECTOR('',#11536,1.);
#3295=VECTOR('',#11539,1.);
#3296=VECTOR('',#11540,1.);
#3297=VECTOR('',#11541,1.);
#3298=VECTOR('',#11544,1.);
#3299=VECTOR('',#11545,1.);
#3300=VECTOR('',#11554,0.576175134594813);
#3301=VECTOR('',#11561,0.576175134594813);
#3302=VECTOR('',#11564,1.);
#3303=VECTOR('',#11565,1.);
#3304=VECTOR('',#11568,1.);
#3305=VECTOR('',#11571,1.);
#3306=VECTOR('',#11576,0.3);
#3307=VECTOR('',#11581,1.);
#3308=VECTOR('',#11584,1.);
#3309=VECTOR('',#11599,0.165);
#3310=VECTOR('',#11606,1.);
#3311=VECTOR('',#11607,1.);
#3312=VECTOR('',#11608,1.);
#3313=VECTOR('',#11609,1.);
#3314=VECTOR('',#11614,1.);
#3315=VECTOR('',#11615,1.);
#3316=VECTOR('',#11618,1.);
#3317=VECTOR('',#11619,1.);
#3318=VECTOR('',#11620,1.);
#3319=VECTOR('',#11623,1.);
#3320=VECTOR('',#11642,0.8);
#3321=VECTOR('',#11645,0.6);
#3322=VECTOR('',#11652,0.6);
#3323=VECTOR('',#11663,0.605);
#3324=VECTOR('',#11670,0.8);
#3325=VECTOR('',#11681,1.);
#3326=VECTOR('',#11688,0.21);
#3327=VECTOR('',#11693,1.);
#3328=VECTOR('',#11698,0.605);
#3329=VECTOR('',#11705,1.1);
#3330=VECTOR('',#11716,1.);
#3331=VECTOR('',#11717,1.);
#3332=VECTOR('',#11718,1.);
#3333=VECTOR('',#11719,1.);
#3334=VECTOR('',#11722,1.);
#3335=VECTOR('',#11723,1.);
#3336=VECTOR('',#11724,1.);
#3337=VECTOR('',#11727,1.);
#3338=VECTOR('',#11728,1.);
#3339=VECTOR('',#11729,1.);
#3340=VECTOR('',#11748,3.);
#3341=VECTOR('',#11751,1.2);
#3342=VECTOR('',#11762,0.605);
#3343=VECTOR('',#11769,3.);
#3344=VECTOR('',#11782,0.225);
#3345=VECTOR('',#11789,0.9);
#3346=VECTOR('',#11806,0.325);
#3347=VECTOR('',#11811,0.35);
#3348=VECTOR('',#11816,0.335);
#3349=VECTOR('',#11825,0.21);
#3350=VECTOR('',#11830,0.2);
#3351=VECTOR('',#11835,0.18);
#3352=VECTOR('',#11840,1.);
#3353=VECTOR('',#11841,1.);
#3354=VECTOR('',#11842,1.);
#3355=VECTOR('',#11843,1.);
#3356=VECTOR('',#11846,1.);
#3357=VECTOR('',#11847,1.);
#3358=VECTOR('',#11848,1.);
#3359=VECTOR('',#11851,1.);
#3360=VECTOR('',#11852,1.);
#3361=VECTOR('',#11853,1.);
#3362=VECTOR('',#11856,1.);
#3363=VECTOR('',#11857,1.);
#3364=VECTOR('',#11858,1.);
#3365=VECTOR('',#11861,1.);
#3366=VECTOR('',#11862,1.);
#3367=VECTOR('',#11863,1.);
#3368=VECTOR('',#11866,1.);
#3369=VECTOR('',#11867,1.);
#3370=VECTOR('',#12032,1.);
#3371=VECTOR('',#12033,1.);
#3372=VECTOR('',#12034,1.);
#3373=VECTOR('',#12035,1.);
#3374=VECTOR('',#12040,1.);
#3375=VECTOR('',#12041,1.);
#3376=VECTOR('',#12044,1.);
#3377=VECTOR('',#12045,1.);
#3378=VECTOR('',#12048,1.);
#3379=VECTOR('',#12049,1.);
#3380=VECTOR('',#12068,0.8);
#3381=VECTOR('',#12071,0.6);
#3382=VECTOR('',#12078,0.6);
#3383=VECTOR('',#12087,1.);
#3384=VECTOR('',#12088,1.);
#3385=VECTOR('',#12089,1.);
#3386=VECTOR('',#12090,1.);
#3387=VECTOR('',#12093,1.);
#3388=VECTOR('',#12094,1.);
#3389=VECTOR('',#12095,1.);
#3390=VECTOR('',#12098,1.);
#3391=VECTOR('',#12099,1.);
#3392=VECTOR('',#12100,1.);
#3393=VECTOR('',#12119,2.9);
#3394=VECTOR('',#12124,1.2);
#3395=VECTOR('',#12133,2.9);
#3396=VECTOR('',#12140,3.);
#3397=VECTOR('',#12153,0.605);
#3398=VECTOR('',#12160,0.8);
#3399=VECTOR('',#12171,1.);
#3400=VECTOR('',#12178,0.21);
#3401=VECTOR('',#12181,1.);
#3402=VECTOR('',#12186,0.605);
#3403=VECTOR('',#12187,0.605);
#3404=VECTOR('',#12194,1.1);
#3405=VECTOR('',#12195,1.1);
#3406=VECTOR('',#12206,1.);
#3407=VECTOR('',#12213,0.21);
#3408=VECTOR('',#12216,1.);
#3409=VECTOR('',#12221,0.605);
#3410=VECTOR('',#12222,0.605);
#3411=VECTOR('',#12229,1.1);
#3412=VECTOR('',#12230,1.1);
#3413=VECTOR('',#12241,1.);
#3414=VECTOR('',#12242,1.);
#3415=VECTOR('',#12243,1.);
#3416=VECTOR('',#12244,1.);
#3417=VECTOR('',#12245,1.);
#3418=VECTOR('',#12246,1.);
#3419=VECTOR('',#12247,1.);
#3420=VECTOR('',#12248,1.);
#3421=VECTOR('',#12251,1.);
#3422=VECTOR('',#12252,1.);
#3423=VECTOR('',#12253,1.);
#3424=VECTOR('',#12256,1.);
#3425=VECTOR('',#12257,1.);
#3426=VECTOR('',#12260,1.);
#3427=VECTOR('',#12261,1.);
#3428=VECTOR('',#12264,1.);
#3429=VECTOR('',#12265,1.);
#3430=VECTOR('',#12268,1.);
#3431=VECTOR('',#12269,1.);
#3432=VECTOR('',#12270,1.);
#3433=VECTOR('',#12271,1.);
#3434=VECTOR('',#12274,1.);
#3435=VECTOR('',#12277,1.);
#3436=VECTOR('',#12280,1.);
#3437=VECTOR('',#12291,1.);
#3438=VECTOR('',#12292,1.);
#3439=VECTOR('',#12293,1.);
#3440=VECTOR('',#12294,1.);
#3441=VECTOR('',#12297,1.);
#3442=VECTOR('',#12298,1.);
#3443=VECTOR('',#12299,1.);
#3444=VECTOR('',#12302,1.);
#3445=VECTOR('',#12303,1.);
#3446=VECTOR('',#12304,1.);
#3447=VECTOR('',#12307,1.);
#3448=VECTOR('',#12308,1.);
#3449=VECTOR('',#12309,1.);
#3450=VECTOR('',#12312,1.);
#3451=VECTOR('',#12313,1.);
#3452=VECTOR('',#12314,1.);
#3453=VECTOR('',#12317,1.);
#3454=VECTOR('',#12318,1.);
#3455=VECTOR('',#12329,0.235);
#3456=VECTOR('',#12332,0.25);
#3457=CIRCLE('',#8746,0.165);
#3458=CIRCLE('',#8747,0.165);
#3459=CIRCLE('',#8749,0.165);
#3460=CIRCLE('',#8750,0.165);
#3461=CIRCLE('',#8752,0.165);
#3462=CIRCLE('',#8753,0.165);
#3463=CIRCLE('',#8755,0.165);
#3464=CIRCLE('',#8756,0.165);
#3465=CIRCLE('',#8758,0.165);
#3466=CIRCLE('',#8759,0.165);
#3467=CIRCLE('',#8761,0.165);
#3468=CIRCLE('',#8762,0.165);
#3469=CIRCLE('',#8764,0.210000000000001);
#3470=CIRCLE('',#8765,0.210000000000001);
#3471=CIRCLE('',#8767,0.21);
#3472=CIRCLE('',#8768,0.21);
#3473=CIRCLE('',#8770,0.21);
#3474=CIRCLE('',#8771,0.21);
#3475=CIRCLE('',#8773,0.210000000000001);
#3476=CIRCLE('',#8774,0.210000000000001);
#3477=CIRCLE('',#8797,0.165);
#3478=CIRCLE('',#8798,0.165);
#3479=CIRCLE('',#8800,0.165);
#3480=CIRCLE('',#8801,0.165);
#3481=CIRCLE('',#8803,0.165);
#3482=CIRCLE('',#8804,0.165);
#3483=CIRCLE('',#8806,0.165);
#3484=CIRCLE('',#8807,0.165);
#3485=CIRCLE('',#8809,0.275);
#3486=CIRCLE('',#8810,0.275);
#3487=CIRCLE('',#8812,0.275);
#3488=CIRCLE('',#8813,0.275);
#3489=CIRCLE('',#8815,0.275);
#3490=CIRCLE('',#8816,0.275);
#3491=CIRCLE('',#8817,0.275);
#3492=CIRCLE('',#8818,0.275);
#3493=CIRCLE('',#8819,0.275);
#3494=CIRCLE('',#8820,0.275);
#3495=CIRCLE('',#8824,0.275);
#3496=CIRCLE('',#8826,0.275);
#3497=CIRCLE('',#8830,0.275);
#3498=CIRCLE('',#8832,0.275);
#3499=CIRCLE('',#8836,0.275);
#3500=CIRCLE('',#8838,0.275);
#3501=CIRCLE('',#8848,0.165);
#3502=CIRCLE('',#8849,0.165);
#3503=CIRCLE('',#8851,0.165);
#3504=CIRCLE('',#8852,0.165);
#3505=CIRCLE('',#8854,0.165);
#3506=CIRCLE('',#8855,0.165);
#3507=CIRCLE('',#8857,0.165);
#3508=CIRCLE('',#8858,0.165);
#3509=CIRCLE('',#8860,1.6);
#3510=CIRCLE('',#8861,1.6);
#3511=CIRCLE('',#8863,0.225);
#3512=CIRCLE('',#8864,0.225);
#3513=CIRCLE('',#8866,0.225);
#3514=CIRCLE('',#8867,0.225);
#3515=CIRCLE('',#8880,0.225);
#3516=CIRCLE('',#8881,0.225);
#3517=CIRCLE('',#8883,0.225);
#3518=CIRCLE('',#8884,0.225);
#3519=CIRCLE('',#8886,0.225);
#3520=CIRCLE('',#8887,0.225);
#3521=CIRCLE('',#8889,0.225);
#3522=CIRCLE('',#8890,0.225);
#3523=CIRCLE('',#8892,1.59);
#3524=CIRCLE('',#8893,1.59);
#3525=CIRCLE('',#8895,1.2);
#3526=CIRCLE('',#8897,1.2);
#3527=CIRCLE('',#8899,2.4);
#3528=CIRCLE('',#8900,2.4);
#3529=CIRCLE('',#8905,0.225);
#3530=CIRCLE('',#8906,0.225);
#3531=CIRCLE('',#8908,0.225);
#3532=CIRCLE('',#8909,0.225);
#3533=CIRCLE('',#8911,0.225);
#3534=CIRCLE('',#8912,0.225);
#3535=CIRCLE('',#8914,0.225);
#3536=CIRCLE('',#8915,0.225);
#3537=CIRCLE('',#8917,1.59);
#3538=CIRCLE('',#8918,1.59);
#3539=CIRCLE('',#8920,1.2);
#3540=CIRCLE('',#8922,1.2);
#3541=CIRCLE('',#8924,2.4);
#3542=CIRCLE('',#8925,2.4);
#3543=CIRCLE('',#8930,0.165);
#3544=CIRCLE('',#8931,0.165);
#3545=CIRCLE('',#8933,0.165);
#3546=CIRCLE('',#8934,0.165);
#3547=CIRCLE('',#8936,0.165);
#3548=CIRCLE('',#8937,0.165);
#3549=CIRCLE('',#8939,0.165);
#3550=CIRCLE('',#8940,0.165);
#3551=CIRCLE('',#8942,1.6);
#3552=CIRCLE('',#8943,1.6);
#3553=CIRCLE('',#8945,0.225);
#3554=CIRCLE('',#8946,0.225);
#3555=CIRCLE('',#8948,0.225);
#3556=CIRCLE('',#8949,0.225);
#3557=CIRCLE('',#8962,0.225);
#3558=CIRCLE('',#8963,0.225);
#3559=CIRCLE('',#8965,0.225);
#3560=CIRCLE('',#8966,0.225);
#3561=CIRCLE('',#8968,0.225);
#3562=CIRCLE('',#8969,0.225);
#3563=CIRCLE('',#8971,0.225);
#3564=CIRCLE('',#8972,0.225);
#3565=CIRCLE('',#8974,1.59);
#3566=CIRCLE('',#8975,1.59);
#3567=CIRCLE('',#8977,1.2);
#3568=CIRCLE('',#8979,1.2);
#3569=CIRCLE('',#8981,2.4);
#3570=CIRCLE('',#8982,2.4);
#3571=CIRCLE('',#8987,0.225);
#3572=CIRCLE('',#8988,0.225);
#3573=CIRCLE('',#8990,0.225);
#3574=CIRCLE('',#8991,0.225);
#3575=CIRCLE('',#8993,0.225);
#3576=CIRCLE('',#8994,0.225);
#3577=CIRCLE('',#8996,0.225);
#3578=CIRCLE('',#8997,0.225);
#3579=CIRCLE('',#8999,1.59);
#3580=CIRCLE('',#9000,1.59);
#3581=CIRCLE('',#9002,1.2);
#3582=CIRCLE('',#9004,1.2);
#3583=CIRCLE('',#9006,2.4);
#3584=CIRCLE('',#9007,2.4);
#3585=CIRCLE('',#9012,0.165);
#3586=CIRCLE('',#9013,0.165);
#3587=CIRCLE('',#9015,0.164999999999999);
#3588=CIRCLE('',#9016,0.164999999999999);
#3589=CIRCLE('',#9018,0.164999999999999);
#3590=CIRCLE('',#9019,0.164999999999999);
#3591=CIRCLE('',#9021,0.165);
#3592=CIRCLE('',#9022,0.165);
#3593=CIRCLE('',#9024,1.6);
#3594=CIRCLE('',#9025,1.6);
#3595=CIRCLE('',#9027,0.225);
#3596=CIRCLE('',#9028,0.225);
#3597=CIRCLE('',#9030,0.225);
#3598=CIRCLE('',#9031,0.225);
#3599=CIRCLE('',#9044,0.225);
#3600=CIRCLE('',#9045,0.225);
#3601=CIRCLE('',#9047,0.225);
#3602=CIRCLE('',#9048,0.225);
#3603=CIRCLE('',#9050,0.225);
#3604=CIRCLE('',#9051,0.225);
#3605=CIRCLE('',#9053,0.225);
#3606=CIRCLE('',#9054,0.225);
#3607=CIRCLE('',#9056,1.59);
#3608=CIRCLE('',#9057,1.59);
#3609=CIRCLE('',#9059,1.2);
#3610=CIRCLE('',#9061,1.2);
#3611=CIRCLE('',#9063,2.4);
#3612=CIRCLE('',#9064,2.4);
#3613=CIRCLE('',#9069,0.225);
#3614=CIRCLE('',#9070,0.225);
#3615=CIRCLE('',#9072,0.225);
#3616=CIRCLE('',#9073,0.225);
#3617=CIRCLE('',#9075,0.225);
#3618=CIRCLE('',#9076,0.225);
#3619=CIRCLE('',#9078,0.225);
#3620=CIRCLE('',#9079,0.225);
#3621=CIRCLE('',#9081,1.59);
#3622=CIRCLE('',#9082,1.59);
#3623=CIRCLE('',#9084,1.2);
#3624=CIRCLE('',#9086,1.2);
#3625=CIRCLE('',#9088,2.4);
#3626=CIRCLE('',#9089,2.4);
#3627=CIRCLE('',#9094,0.165);
#3628=CIRCLE('',#9095,0.165);
#3629=CIRCLE('',#9097,0.164999999999999);
#3630=CIRCLE('',#9098,0.164999999999999);
#3631=CIRCLE('',#9100,0.164999999999999);
#3632=CIRCLE('',#9101,0.164999999999999);
#3633=CIRCLE('',#9103,0.165);
#3634=CIRCLE('',#9104,0.165);
#3635=CIRCLE('',#9106,1.6);
#3636=CIRCLE('',#9107,1.6);
#3637=CIRCLE('',#9109,0.225);
#3638=CIRCLE('',#9110,0.225);
#3639=CIRCLE('',#9112,0.225);
#3640=CIRCLE('',#9113,0.225);
#3641=CIRCLE('',#9126,0.225);
#3642=CIRCLE('',#9127,0.225);
#3643=CIRCLE('',#9129,0.225);
#3644=CIRCLE('',#9130,0.225);
#3645=CIRCLE('',#9132,0.225);
#3646=CIRCLE('',#9133,0.225);
#3647=CIRCLE('',#9135,0.225);
#3648=CIRCLE('',#9136,0.225);
#3649=CIRCLE('',#9138,1.59);
#3650=CIRCLE('',#9139,1.59);
#3651=CIRCLE('',#9141,1.2);
#3652=CIRCLE('',#9143,1.2);
#3653=CIRCLE('',#9145,2.4);
#3654=CIRCLE('',#9146,2.4);
#3655=CIRCLE('',#9151,0.225);
#3656=CIRCLE('',#9152,0.225);
#3657=CIRCLE('',#9154,0.225);
#3658=CIRCLE('',#9155,0.225);
#3659=CIRCLE('',#9157,0.225);
#3660=CIRCLE('',#9158,0.225);
#3661=CIRCLE('',#9160,0.225);
#3662=CIRCLE('',#9161,0.225);
#3663=CIRCLE('',#9163,1.59);
#3664=CIRCLE('',#9164,1.59);
#3665=CIRCLE('',#9166,1.2);
#3666=CIRCLE('',#9168,1.2);
#3667=CIRCLE('',#9170,2.4);
#3668=CIRCLE('',#9171,2.4);
#3669=CIRCLE('',#9176,0.25);
#3670=CIRCLE('',#9177,0.25);
#3671=CIRCLE('',#9179,0.25);
#3672=CIRCLE('',#9180,0.25);
#3673=CIRCLE('',#9182,0.4);
#3674=CIRCLE('',#9183,0.4);
#3675=CIRCLE('',#9185,0.225);
#3676=CIRCLE('',#9187,0.225);
#3677=CIRCLE('',#9189,0.4);
#3678=CIRCLE('',#9190,0.4);
#3679=CIRCLE('',#9192,0.225);
#3680=CIRCLE('',#9194,0.225);
#3681=CIRCLE('',#9203,0.7);
#3682=CIRCLE('',#9204,0.7);
#3683=CIRCLE('',#9209,0.7);
#3684=CIRCLE('',#9210,0.7);
#3685=CIRCLE('',#9214,0.05);
#3686=CIRCLE('',#9215,0.05);
#3687=CIRCLE('',#9220,0.7);
#3688=CIRCLE('',#9221,0.7);
#3689=CIRCLE('',#9226,0.7);
#3690=CIRCLE('',#9227,0.7);
#3691=CIRCLE('',#9231,0.05);
#3692=CIRCLE('',#9232,0.05);
#3693=CIRCLE('',#9237,0.375);
#3694=CIRCLE('',#9239,0.425);
#3695=CIRCLE('',#9241,0.425);
#3696=CIRCLE('',#9243,0.395);
#3697=CIRCLE('',#9245,0.27);
#3698=CIRCLE('',#9247,0.24505);
#3699=CIRCLE('',#9249,0.24505);
#3700=CIRCLE('',#9251,0.2);
#3701=CIRCLE('',#9264,1.070235);
#3702=CIRCLE('',#9265,1.070235);
#3703=CIRCLE('',#9266,0.309556);
#3704=CIRCLE('',#9267,1.070235);
#3705=CIRCLE('',#9268,1.070235);
#3706=CIRCLE('',#9270,1.070235);
#3707=CIRCLE('',#9272,0.6);
#3708=CIRCLE('',#9273,0.6);
#3709=CIRCLE('',#9275,0.66);
#3710=CIRCLE('',#9278,1.070235);
#3711=CIRCLE('',#9280,0.66);
#3712=CIRCLE('',#9284,1.129765);
#3713=CIRCLE('',#9285,1.129765);
#3714=CIRCLE('',#9286,0.309556);
#3715=CIRCLE('',#9287,1.129765);
#3716=CIRCLE('',#9288,1.129765);
#3717=CIRCLE('',#9290,1.129765);
#3718=CIRCLE('',#9292,1.54);
#3719=CIRCLE('',#9293,1.129765);
#3720=CIRCLE('',#9295,1.6);
#3721=CIRCLE('',#9297,1.6);
#3722=CIRCLE('',#9299,1.54);
#3723=CIRCLE('',#9304,0.29765);
#3724=CIRCLE('',#9306,0.29765);
#3725=CIRCLE('',#9308,0.29765);
#3726=CIRCLE('',#9310,0.29765);
#3727=CIRCLE('',#9312,0.29765);
#3728=CIRCLE('',#9314,0.29765);
#3729=CIRCLE('',#9316,0.29765);
#3730=CIRCLE('',#9319,0.303778037777585);
#3731=CIRCLE('',#9320,0.303778037777585);
#3732=CIRCLE('',#9322,1.123812);
#3733=CIRCLE('',#9323,1.123812);
#3734=CIRCLE('',#9324,1.123812);
#3735=CIRCLE('',#9325,1.123812);
#3736=CIRCLE('',#9326,1.123812);
#3737=CIRCLE('',#9327,1.123812);
#3738=CIRCLE('',#9328,1.123812);
#3739=CIRCLE('',#9329,1.123812);
#3740=CIRCLE('',#9330,1.123812);
#3741=CIRCLE('',#9332,1.076188);
#3742=CIRCLE('',#9333,0.303778037777585);
#3743=CIRCLE('',#9335,0.303778037777585);
#3744=CIRCLE('',#9337,1.076188);
#3745=CIRCLE('',#9338,0.303778037777585);
#3746=CIRCLE('',#9340,0.303778037777585);
#3747=CIRCLE('',#9342,1.076188);
#3748=CIRCLE('',#9343,1.076188);
#3749=CIRCLE('',#9344,0.303778037777585);
#3750=CIRCLE('',#9346,0.303778037777585);
#3751=CIRCLE('',#9348,1.076188);
#3752=CIRCLE('',#9349,0.303778037777585);
#3753=CIRCLE('',#9351,0.303778037777585);
#3754=CIRCLE('',#9353,1.076188);
#3755=CIRCLE('',#9354,0.303778037777585);
#3756=CIRCLE('',#9356,0.303778037777585);
#3757=CIRCLE('',#9358,1.076188);
#3758=CIRCLE('',#9359,1.076188);
#3759=CIRCLE('',#9360,1.076188);
#3760=CIRCLE('',#9362,0.303778037777585);
#3761=CIRCLE('',#9364,0.303778037777585);
#3762=CIRCLE('',#9369,1.119765);
#3763=CIRCLE('',#9370,1.085235);
#3764=CIRCLE('',#9372,1.119765);
#3765=CIRCLE('',#9374,1.085235);
#3766=CIRCLE('',#9377,1.119765);
#3767=CIRCLE('',#9378,1.085235);
#3768=CIRCLE('',#9380,1.119765);
#3769=CIRCLE('',#9382,1.085235);
#3770=CIRCLE('',#9399,0.1954);
#3771=CIRCLE('',#9401,0.3);
#3772=CIRCLE('',#9403,0.35);
#3773=CIRCLE('',#9405,0.35);
#3774=CIRCLE('',#9407,0.32);
#3775=CIRCLE('',#9409,0.22);
#3776=CIRCLE('',#9411,0.1954);
#3777=CIRCLE('',#9415,0.45);
#3778=CIRCLE('',#9417,0.5);
#3779=CIRCLE('',#9419,0.5);
#3780=CIRCLE('',#9421,0.47);
#3781=CIRCLE('',#9423,0.32);
#3782=CIRCLE('',#9425,0.2942);
#3783=CIRCLE('',#9427,0.2942);
#3784=CIRCLE('',#9429,0.24);
#3785=CIRCLE('',#9441,0.475);
#3786=CIRCLE('',#9443,0.475);
#3787=CIRCLE('',#9448,0.25175);
#3788=CIRCLE('',#9449,0.25175);
#3789=CIRCLE('',#9458,0.165);
#3790=CIRCLE('',#9459,0.165);
#3791=CIRCLE('',#9463,0.6);
#3792=CIRCLE('',#9467,0.6);
#3793=CIRCLE('',#9469,0.8);
#3794=CIRCLE('',#9470,0.6);
#3795=CIRCLE('',#9472,0.8);
#3796=CIRCLE('',#9473,0.6);
#3797=CIRCLE('',#9476,0.6);
#3798=CIRCLE('',#9478,0.6);
#3799=CIRCLE('',#9483,0.605);
#3800=CIRCLE('',#9484,0.605);
#3801=CIRCLE('',#9486,0.8);
#3802=CIRCLE('',#9487,0.8);
#3803=CIRCLE('',#9492,0.21);
#3804=CIRCLE('',#9494,0.21);
#3805=CIRCLE('',#9495,0.21);
#3806=CIRCLE('',#9498,0.605);
#3807=CIRCLE('',#9499,0.605);
#3808=CIRCLE('',#9501,1.1);
#3809=CIRCLE('',#9502,1.1);
#3810=CIRCLE('',#9510,3.);
#3811=CIRCLE('',#9511,0.6);
#3812=CIRCLE('',#9513,0.6);
#3813=CIRCLE('',#9515,3.);
#3814=CIRCLE('',#9516,1.2);
#3815=CIRCLE('',#9519,1.2);
#3816=CIRCLE('',#9523,0.605);
#3817=CIRCLE('',#9524,0.605);
#3818=CIRCLE('',#9526,3.);
#3819=CIRCLE('',#9527,3.);
#3820=CIRCLE('',#9532,0.225);
#3821=CIRCLE('',#9533,0.225);
#3822=CIRCLE('',#9535,0.9);
#3823=CIRCLE('',#9536,0.9);
#3824=CIRCLE('',#9541,0.3);
#3825=CIRCLE('',#9543,0.35);
#3826=CIRCLE('',#9545,0.35);
#3827=CIRCLE('',#9547,0.32);
#3828=CIRCLE('',#9549,0.22);
#3829=CIRCLE('',#9551,0.1954);
#3830=CIRCLE('',#9553,0.1954);
#3831=CIRCLE('',#9555,0.16);
#3832=CIRCLE('',#9646,0.6);
#3833=CIRCLE('',#9650,0.6);
#3834=CIRCLE('',#9652,0.8);
#3835=CIRCLE('',#9653,0.6);
#3836=CIRCLE('',#9655,0.8);
#3837=CIRCLE('',#9656,0.6);
#3838=CIRCLE('',#9659,0.6);
#3839=CIRCLE('',#9661,0.6);
#3840=CIRCLE('',#9669,1.2);
#3841=CIRCLE('',#9670,0.6);
#3842=CIRCLE('',#9672,0.6);
#3843=CIRCLE('',#9674,2.9);
#3844=CIRCLE('',#9675,1.2);
#3845=CIRCLE('',#9677,2.9);
#3846=CIRCLE('',#9682,2.9);
#3847=CIRCLE('',#9683,2.9);
#3848=CIRCLE('',#9685,3.);
#3849=CIRCLE('',#9686,3.);
#3850=CIRCLE('',#9691,0.605);
#3851=CIRCLE('',#9692,0.605);
#3852=CIRCLE('',#9694,0.8);
#3853=CIRCLE('',#9695,0.8);
#3854=CIRCLE('',#9700,0.21);
#3855=CIRCLE('',#9702,0.21);
#3856=CIRCLE('',#9705,0.605);
#3857=CIRCLE('',#9706,0.605);
#3858=CIRCLE('',#9708,1.1);
#3859=CIRCLE('',#9709,1.1);
#3860=CIRCLE('',#9714,0.21);
#3861=CIRCLE('',#9716,0.21);
#3862=CIRCLE('',#9719,0.605);
#3863=CIRCLE('',#9720,0.605);
#3864=CIRCLE('',#9722,1.1);
#3865=CIRCLE('',#9723,1.1);
#3866=CIRCLE('',#9739,0.24505);
#3867=CIRCLE('',#9748,0.22);
#3868=CIRCLE('',#9750,0.24505);
#3869=VERTEX_POINT('',#12379);
#3870=VERTEX_POINT('',#12381);
#3871=VERTEX_POINT('',#12385);
#3872=VERTEX_POINT('',#12387);
#3873=VERTEX_POINT('',#12391);
#3874=VERTEX_POINT('',#12393);
#3875=VERTEX_POINT('',#12397);
#3876=VERTEX_POINT('',#12399);
#3877=VERTEX_POINT('',#12403);
#3878=VERTEX_POINT('',#12405);
#3879=VERTEX_POINT('',#12409);
#3880=VERTEX_POINT('',#12411);
#3881=VERTEX_POINT('',#12415);
#3882=VERTEX_POINT('',#12417);
#3883=VERTEX_POINT('',#12421);
#3884=VERTEX_POINT('',#12423);
#3885=VERTEX_POINT('',#12427);
#3886=VERTEX_POINT('',#12429);
#3887=VERTEX_POINT('',#12433);
#3888=VERTEX_POINT('',#12435);
#3889=VERTEX_POINT('',#12439);
#3890=VERTEX_POINT('',#12440);
#3891=VERTEX_POINT('',#12442);
#3892=VERTEX_POINT('',#12444);
#3893=VERTEX_POINT('',#12448);
#3894=VERTEX_POINT('',#12450);
#3895=VERTEX_POINT('',#12454);
#3896=VERTEX_POINT('',#12456);
#3897=VERTEX_POINT('',#12466);
#3898=VERTEX_POINT('',#12467);
#3899=VERTEX_POINT('',#12469);
#3900=VERTEX_POINT('',#12471);
#3901=VERTEX_POINT('',#12475);
#3902=VERTEX_POINT('',#12477);
#3903=VERTEX_POINT('',#12481);
#3904=VERTEX_POINT('',#12483);
#3905=VERTEX_POINT('',#12493);
#3906=VERTEX_POINT('',#12494);
#3907=VERTEX_POINT('',#12496);
#3908=VERTEX_POINT('',#12498);
#3909=VERTEX_POINT('',#12502);
#3910=VERTEX_POINT('',#12504);
#3911=VERTEX_POINT('',#12508);
#3912=VERTEX_POINT('',#12510);
#3913=VERTEX_POINT('',#12520);
#3914=VERTEX_POINT('',#12522);
#3915=VERTEX_POINT('',#12526);
#3916=VERTEX_POINT('',#12528);
#3917=VERTEX_POINT('',#12532);
#3918=VERTEX_POINT('',#12534);
#3919=VERTEX_POINT('',#12538);
#3920=VERTEX_POINT('',#12540);
#3921=VERTEX_POINT('',#12544);
#3922=VERTEX_POINT('',#12545);
#3923=VERTEX_POINT('',#12547);
#3924=VERTEX_POINT('',#12549);
#3925=VERTEX_POINT('',#12553);
#3926=VERTEX_POINT('',#12554);
#3927=VERTEX_POINT('',#12556);
#3928=VERTEX_POINT('',#12558);
#3929=VERTEX_POINT('',#12562);
#3930=VERTEX_POINT('',#12563);
#3931=VERTEX_POINT('',#12565);
#3932=VERTEX_POINT('',#12567);
#3933=VERTEX_POINT('',#12572);
#3934=VERTEX_POINT('',#12573);
#3935=VERTEX_POINT('',#12575);
#3936=VERTEX_POINT('',#12577);
#3937=VERTEX_POINT('',#12580);
#3938=VERTEX_POINT('',#12581);
#3939=VERTEX_POINT('',#12583);
#3940=VERTEX_POINT('',#12585);
#3941=VERTEX_POINT('',#12588);
#3942=VERTEX_POINT('',#12589);
#3943=VERTEX_POINT('',#12591);
#3944=VERTEX_POINT('',#12593);
#3945=VERTEX_POINT('',#12601);
#3946=VERTEX_POINT('',#12603);
#3947=VERTEX_POINT('',#12607);
#3948=VERTEX_POINT('',#12609);
#3949=VERTEX_POINT('',#12617);
#3950=VERTEX_POINT('',#12619);
#3951=VERTEX_POINT('',#12623);
#3952=VERTEX_POINT('',#12625);
#3953=VERTEX_POINT('',#12633);
#3954=VERTEX_POINT('',#12635);
#3955=VERTEX_POINT('',#12639);
#3956=VERTEX_POINT('',#12641);
#3957=VERTEX_POINT('',#12649);
#3958=VERTEX_POINT('',#12650);
#3959=VERTEX_POINT('',#12655);
#3960=VERTEX_POINT('',#12659);
#3961=VERTEX_POINT('',#12667);
#3962=VERTEX_POINT('',#12669);
#3963=VERTEX_POINT('',#12673);
#3964=VERTEX_POINT('',#12675);
#3965=VERTEX_POINT('',#12679);
#3966=VERTEX_POINT('',#12681);
#3967=VERTEX_POINT('',#12685);
#3968=VERTEX_POINT('',#12687);
#3969=VERTEX_POINT('',#12691);
#3970=VERTEX_POINT('',#12693);
#3971=VERTEX_POINT('',#12697);
#3972=VERTEX_POINT('',#12699);
#3973=VERTEX_POINT('',#12703);
#3974=VERTEX_POINT('',#12705);
#3975=VERTEX_POINT('',#12709);
#3976=VERTEX_POINT('',#12710);
#3977=VERTEX_POINT('',#12712);
#3978=VERTEX_POINT('',#12714);
#3979=VERTEX_POINT('',#12718);
#3980=VERTEX_POINT('',#12719);
#3981=VERTEX_POINT('',#12721);
#3982=VERTEX_POINT('',#12723);
#3983=VERTEX_POINT('',#12727);
#3984=VERTEX_POINT('',#12729);
#3985=VERTEX_POINT('',#12733);
#3986=VERTEX_POINT('',#12735);
#3987=VERTEX_POINT('',#12739);
#3988=VERTEX_POINT('',#12741);
#3989=VERTEX_POINT('',#12746);
#3990=VERTEX_POINT('',#12750);
#3991=VERTEX_POINT('',#12760);
#3992=VERTEX_POINT('',#12762);
#3993=VERTEX_POINT('',#12766);
#3994=VERTEX_POINT('',#12768);
#3995=VERTEX_POINT('',#12772);
#3996=VERTEX_POINT('',#12774);
#3997=VERTEX_POINT('',#12778);
#3998=VERTEX_POINT('',#12780);
#3999=VERTEX_POINT('',#12784);
#4000=VERTEX_POINT('',#12786);
#4001=VERTEX_POINT('',#12790);
#4002=VERTEX_POINT('',#12793);
#4003=VERTEX_POINT('',#12797);
#4004=VERTEX_POINT('',#12799);
#4005=VERTEX_POINT('',#12806);
#4006=VERTEX_POINT('',#12808);
#4007=VERTEX_POINT('',#12812);
#4008=VERTEX_POINT('',#12814);
#4009=VERTEX_POINT('',#12818);
#4010=VERTEX_POINT('',#12820);
#4011=VERTEX_POINT('',#12824);
#4012=VERTEX_POINT('',#12826);
#4013=VERTEX_POINT('',#12830);
#4014=VERTEX_POINT('',#12832);
#4015=VERTEX_POINT('',#12836);
#4016=VERTEX_POINT('',#12839);
#4017=VERTEX_POINT('',#12843);
#4018=VERTEX_POINT('',#12845);
#4019=VERTEX_POINT('',#12852);
#4020=VERTEX_POINT('',#12854);
#4021=VERTEX_POINT('',#12858);
#4022=VERTEX_POINT('',#12860);
#4023=VERTEX_POINT('',#12864);
#4024=VERTEX_POINT('',#12866);
#4025=VERTEX_POINT('',#12870);
#4026=VERTEX_POINT('',#12872);
#4027=VERTEX_POINT('',#12876);
#4028=VERTEX_POINT('',#12878);
#4029=VERTEX_POINT('',#12882);
#4030=VERTEX_POINT('',#12884);
#4031=VERTEX_POINT('',#12888);
#4032=VERTEX_POINT('',#12890);
#4033=VERTEX_POINT('',#12894);
#4034=VERTEX_POINT('',#12895);
#4035=VERTEX_POINT('',#12897);
#4036=VERTEX_POINT('',#12899);
#4037=VERTEX_POINT('',#12903);
#4038=VERTEX_POINT('',#12904);
#4039=VERTEX_POINT('',#12906);
#4040=VERTEX_POINT('',#12908);
#4041=VERTEX_POINT('',#12912);
#4042=VERTEX_POINT('',#12914);
#4043=VERTEX_POINT('',#12918);
#4044=VERTEX_POINT('',#12920);
#4045=VERTEX_POINT('',#12924);
#4046=VERTEX_POINT('',#12926);
#4047=VERTEX_POINT('',#12931);
#4048=VERTEX_POINT('',#12935);
#4049=VERTEX_POINT('',#12945);
#4050=VERTEX_POINT('',#12947);
#4051=VERTEX_POINT('',#12951);
#4052=VERTEX_POINT('',#12953);
#4053=VERTEX_POINT('',#12957);
#4054=VERTEX_POINT('',#12959);
#4055=VERTEX_POINT('',#12963);
#4056=VERTEX_POINT('',#12965);
#4057=VERTEX_POINT('',#12969);
#4058=VERTEX_POINT('',#12971);
#4059=VERTEX_POINT('',#12975);
#4060=VERTEX_POINT('',#12978);
#4061=VERTEX_POINT('',#12982);
#4062=VERTEX_POINT('',#12984);
#4063=VERTEX_POINT('',#12991);
#4064=VERTEX_POINT('',#12993);
#4065=VERTEX_POINT('',#12997);
#4066=VERTEX_POINT('',#12999);
#4067=VERTEX_POINT('',#13003);
#4068=VERTEX_POINT('',#13005);
#4069=VERTEX_POINT('',#13009);
#4070=VERTEX_POINT('',#13011);
#4071=VERTEX_POINT('',#13015);
#4072=VERTEX_POINT('',#13017);
#4073=VERTEX_POINT('',#13021);
#4074=VERTEX_POINT('',#13024);
#4075=VERTEX_POINT('',#13028);
#4076=VERTEX_POINT('',#13030);
#4077=VERTEX_POINT('',#13037);
#4078=VERTEX_POINT('',#13039);
#4079=VERTEX_POINT('',#13043);
#4080=VERTEX_POINT('',#13045);
#4081=VERTEX_POINT('',#13049);
#4082=VERTEX_POINT('',#13051);
#4083=VERTEX_POINT('',#13055);
#4084=VERTEX_POINT('',#13057);
#4085=VERTEX_POINT('',#13061);
#4086=VERTEX_POINT('',#13063);
#4087=VERTEX_POINT('',#13067);
#4088=VERTEX_POINT('',#13069);
#4089=VERTEX_POINT('',#13073);
#4090=VERTEX_POINT('',#13075);
#4091=VERTEX_POINT('',#13079);
#4092=VERTEX_POINT('',#13080);
#4093=VERTEX_POINT('',#13082);
#4094=VERTEX_POINT('',#13084);
#4095=VERTEX_POINT('',#13088);
#4096=VERTEX_POINT('',#13089);
#4097=VERTEX_POINT('',#13091);
#4098=VERTEX_POINT('',#13093);
#4099=VERTEX_POINT('',#13097);
#4100=VERTEX_POINT('',#13099);
#4101=VERTEX_POINT('',#13103);
#4102=VERTEX_POINT('',#13105);
#4103=VERTEX_POINT('',#13109);
#4104=VERTEX_POINT('',#13111);
#4105=VERTEX_POINT('',#13116);
#4106=VERTEX_POINT('',#13120);
#4107=VERTEX_POINT('',#13130);
#4108=VERTEX_POINT('',#13132);
#4109=VERTEX_POINT('',#13136);
#4110=VERTEX_POINT('',#13138);
#4111=VERTEX_POINT('',#13142);
#4112=VERTEX_POINT('',#13144);
#4113=VERTEX_POINT('',#13148);
#4114=VERTEX_POINT('',#13150);
#4115=VERTEX_POINT('',#13154);
#4116=VERTEX_POINT('',#13156);
#4117=VERTEX_POINT('',#13160);
#4118=VERTEX_POINT('',#13163);
#4119=VERTEX_POINT('',#13167);
#4120=VERTEX_POINT('',#13169);
#4121=VERTEX_POINT('',#13176);
#4122=VERTEX_POINT('',#13178);
#4123=VERTEX_POINT('',#13182);
#4124=VERTEX_POINT('',#13184);
#4125=VERTEX_POINT('',#13188);
#4126=VERTEX_POINT('',#13190);
#4127=VERTEX_POINT('',#13194);
#4128=VERTEX_POINT('',#13196);
#4129=VERTEX_POINT('',#13200);
#4130=VERTEX_POINT('',#13202);
#4131=VERTEX_POINT('',#13206);
#4132=VERTEX_POINT('',#13209);
#4133=VERTEX_POINT('',#13213);
#4134=VERTEX_POINT('',#13215);
#4135=VERTEX_POINT('',#13222);
#4136=VERTEX_POINT('',#13224);
#4137=VERTEX_POINT('',#13228);
#4138=VERTEX_POINT('',#13230);
#4139=VERTEX_POINT('',#13234);
#4140=VERTEX_POINT('',#13236);
#4141=VERTEX_POINT('',#13240);
#4142=VERTEX_POINT('',#13242);
#4143=VERTEX_POINT('',#13246);
#4144=VERTEX_POINT('',#13248);
#4145=VERTEX_POINT('',#13252);
#4146=VERTEX_POINT('',#13254);
#4147=VERTEX_POINT('',#13258);
#4148=VERTEX_POINT('',#13260);
#4149=VERTEX_POINT('',#13264);
#4150=VERTEX_POINT('',#13265);
#4151=VERTEX_POINT('',#13267);
#4152=VERTEX_POINT('',#13269);
#4153=VERTEX_POINT('',#13273);
#4154=VERTEX_POINT('',#13274);
#4155=VERTEX_POINT('',#13276);
#4156=VERTEX_POINT('',#13278);
#4157=VERTEX_POINT('',#13282);
#4158=VERTEX_POINT('',#13284);
#4159=VERTEX_POINT('',#13288);
#4160=VERTEX_POINT('',#13290);
#4161=VERTEX_POINT('',#13294);
#4162=VERTEX_POINT('',#13296);
#4163=VERTEX_POINT('',#13301);
#4164=VERTEX_POINT('',#13305);
#4165=VERTEX_POINT('',#13315);
#4166=VERTEX_POINT('',#13317);
#4167=VERTEX_POINT('',#13321);
#4168=VERTEX_POINT('',#13323);
#4169=VERTEX_POINT('',#13327);
#4170=VERTEX_POINT('',#13329);
#4171=VERTEX_POINT('',#13333);
#4172=VERTEX_POINT('',#13335);
#4173=VERTEX_POINT('',#13339);
#4174=VERTEX_POINT('',#13341);
#4175=VERTEX_POINT('',#13345);
#4176=VERTEX_POINT('',#13348);
#4177=VERTEX_POINT('',#13352);
#4178=VERTEX_POINT('',#13354);
#4179=VERTEX_POINT('',#13361);
#4180=VERTEX_POINT('',#13363);
#4181=VERTEX_POINT('',#13367);
#4182=VERTEX_POINT('',#13369);
#4183=VERTEX_POINT('',#13373);
#4184=VERTEX_POINT('',#13375);
#4185=VERTEX_POINT('',#13379);
#4186=VERTEX_POINT('',#13381);
#4187=VERTEX_POINT('',#13385);
#4188=VERTEX_POINT('',#13387);
#4189=VERTEX_POINT('',#13391);
#4190=VERTEX_POINT('',#13394);
#4191=VERTEX_POINT('',#13398);
#4192=VERTEX_POINT('',#13400);
#4193=VERTEX_POINT('',#13407);
#4194=VERTEX_POINT('',#13409);
#4195=VERTEX_POINT('',#13413);
#4196=VERTEX_POINT('',#13415);
#4197=VERTEX_POINT('',#13419);
#4198=VERTEX_POINT('',#13421);
#4199=VERTEX_POINT('',#13425);
#4200=VERTEX_POINT('',#13428);
#4201=VERTEX_POINT('',#13432);
#4202=VERTEX_POINT('',#13434);
#4203=VERTEX_POINT('',#13438);
#4204=VERTEX_POINT('',#13441);
#4205=VERTEX_POINT('',#13445);
#4206=VERTEX_POINT('',#13446);
#4207=VERTEX_POINT('',#13448);
#4208=VERTEX_POINT('',#13450);
#4209=VERTEX_POINT('',#13454);
#4210=VERTEX_POINT('',#13456);
#4211=VERTEX_POINT('',#13460);
#4212=VERTEX_POINT('',#13462);
#4213=VERTEX_POINT('',#13472);
#4214=VERTEX_POINT('',#13474);
#4215=VERTEX_POINT('',#13481);
#4216=VERTEX_POINT('',#13483);
#4217=VERTEX_POINT('',#14319);
#4218=VERTEX_POINT('',#14321);
#4219=VERTEX_POINT('',#14410);
#4220=VERTEX_POINT('',#14412);
#4221=VERTEX_POINT('',#14419);
#4222=VERTEX_POINT('',#14421);
#4223=VERTEX_POINT('',#15237);
#4224=VERTEX_POINT('',#15239);
#4225=VERTEX_POINT('',#15326);
#4226=VERTEX_POINT('',#15329);
#4227=VERTEX_POINT('',#15333);
#4228=VERTEX_POINT('',#15337);
#4229=VERTEX_POINT('',#15341);
#4230=VERTEX_POINT('',#15344);
#4231=VERTEX_POINT('',#15348);
#4232=VERTEX_POINT('',#15352);
#4233=VERTEX_POINT('',#15357);
#4234=VERTEX_POINT('',#15358);
#4235=VERTEX_POINT('',#15360);
#4236=VERTEX_POINT('',#15362);
#4237=VERTEX_POINT('',#15366);
#4238=VERTEX_POINT('',#15368);
#4239=VERTEX_POINT('',#15372);
#4240=VERTEX_POINT('',#15374);
#4241=VERTEX_POINT('',#15378);
#4242=VERTEX_POINT('',#15380);
#4243=VERTEX_POINT('',#15384);
#4244=VERTEX_POINT('',#15386);
#4245=VERTEX_POINT('',#15397);
#4246=VERTEX_POINT('',#15398);
#4247=VERTEX_POINT('',#15401);
#4248=VERTEX_POINT('',#15403);
#4249=VERTEX_POINT('',#15407);
#4250=VERTEX_POINT('',#15411);
#4251=VERTEX_POINT('',#15413);
#4252=VERTEX_POINT('',#15417);
#4253=VERTEX_POINT('',#15422);
#4254=VERTEX_POINT('',#15426);
#4255=VERTEX_POINT('',#15432);
#4256=VERTEX_POINT('',#15433);
#4257=VERTEX_POINT('',#15436);
#4258=VERTEX_POINT('',#15438);
#4259=VERTEX_POINT('',#15442);
#4260=VERTEX_POINT('',#15446);
#4261=VERTEX_POINT('',#15448);
#4262=VERTEX_POINT('',#15451);
#4263=VERTEX_POINT('',#15455);
#4264=VERTEX_POINT('',#15459);
#4265=VERTEX_POINT('',#15467);
#4266=VERTEX_POINT('',#15468);
#4267=VERTEX_POINT('',#15471);
#4268=VERTEX_POINT('',#15472);
#4269=VERTEX_POINT('',#15475);
#4270=VERTEX_POINT('',#15476);
#4271=VERTEX_POINT('',#15479);
#4272=VERTEX_POINT('',#15480);
#4273=VERTEX_POINT('',#15483);
#4274=VERTEX_POINT('',#15484);
#4275=VERTEX_POINT('',#15487);
#4276=VERTEX_POINT('',#15488);
#4277=VERTEX_POINT('',#15491);
#4278=VERTEX_POINT('',#15492);
#4279=VERTEX_POINT('',#15496);
#4280=VERTEX_POINT('',#15497);
#4281=VERTEX_POINT('',#15520);
#4282=VERTEX_POINT('',#15522);
#4283=VERTEX_POINT('',#15547);
#4284=VERTEX_POINT('',#15549);
#4285=VERTEX_POINT('',#15572);
#4286=VERTEX_POINT('',#15574);
#4287=VERTEX_POINT('',#15597);
#4288=VERTEX_POINT('',#15599);
#4289=VERTEX_POINT('',#15602);
#4290=VERTEX_POINT('',#15604);
#4291=VERTEX_POINT('',#15627);
#4292=VERTEX_POINT('',#15629);
#4293=VERTEX_POINT('',#15652);
#4294=VERTEX_POINT('',#15654);
#4295=VERTEX_POINT('',#15677);
#4296=VERTEX_POINT('',#15679);
#4297=VERTEX_POINT('',#15704);
#4298=VERTEX_POINT('',#15708);
#4299=VERTEX_POINT('',#15733);
#4300=VERTEX_POINT('',#15737);
#4301=VERTEX_POINT('',#15762);
#4302=VERTEX_POINT('',#15764);
#4303=VERTEX_POINT('',#15768);
#4304=VERTEX_POINT('',#15793);
#4305=VERTEX_POINT('',#15797);
#4306=VERTEX_POINT('',#15822);
#4307=VERTEX_POINT('',#15826);
#4308=VERTEX_POINT('',#15851);
#4309=VERTEX_POINT('',#15854);
#4310=VERTEX_POINT('',#15856);
#4311=VERTEX_POINT('',#15888);
#4312=VERTEX_POINT('',#15890);
#4313=VERTEX_POINT('',#15893);
#4314=VERTEX_POINT('',#15897);
#4315=VERTEX_POINT('',#15902);
#4316=VERTEX_POINT('',#15904);
#4317=VERTEX_POINT('',#15907);
#4318=VERTEX_POINT('',#15911);
#4319=VERTEX_POINT('',#15922);
#4320=VERTEX_POINT('',#15923);
#4321=VERTEX_POINT('',#15925);
#4322=VERTEX_POINT('',#15927);
#4323=VERTEX_POINT('',#15931);
#4324=VERTEX_POINT('',#15933);
#4325=VERTEX_POINT('',#15937);
#4326=VERTEX_POINT('',#15939);
#4327=VERTEX_POINT('',#15943);
#4328=VERTEX_POINT('',#15945);
#4329=VERTEX_POINT('',#15949);
#4330=VERTEX_POINT('',#15951);
#4331=VERTEX_POINT('',#15960);
#4332=VERTEX_POINT('',#15963);
#4333=VERTEX_POINT('',#15966);
#4334=VERTEX_POINT('',#15970);
#4335=VERTEX_POINT('',#15974);
#4336=VERTEX_POINT('',#15978);
#4337=VERTEX_POINT('',#15981);
#4338=VERTEX_POINT('',#15988);
#4339=VERTEX_POINT('',#15991);
#4340=VERTEX_POINT('',#15995);
#4341=VERTEX_POINT('',#15999);
#4342=VERTEX_POINT('',#16003);
#4343=VERTEX_POINT('',#16006);
#4344=VERTEX_POINT('',#16010);
#4345=VERTEX_POINT('',#16014);
#4346=VERTEX_POINT('',#16019);
#4347=VERTEX_POINT('',#16020);
#4348=VERTEX_POINT('',#16022);
#4349=VERTEX_POINT('',#16024);
#4350=VERTEX_POINT('',#16028);
#4351=VERTEX_POINT('',#16030);
#4352=VERTEX_POINT('',#16034);
#4353=VERTEX_POINT('',#16036);
#4354=VERTEX_POINT('',#16040);
#4355=VERTEX_POINT('',#16042);
#4356=VERTEX_POINT('',#16046);
#4357=VERTEX_POINT('',#16048);
#4358=VERTEX_POINT('',#16058);
#4359=VERTEX_POINT('',#16059);
#4360=VERTEX_POINT('',#16063);
#4361=VERTEX_POINT('',#16067);
#4362=VERTEX_POINT('',#16070);
#4363=VERTEX_POINT('',#16074);
#4364=VERTEX_POINT('',#16078);
#4365=VERTEX_POINT('',#16086);
#4366=VERTEX_POINT('',#16088);
#4367=VERTEX_POINT('',#16090);
#4368=VERTEX_POINT('',#16094);
#4369=VERTEX_POINT('',#16098);
#4370=VERTEX_POINT('',#16102);
#4371=VERTEX_POINT('',#16106);
#4372=VERTEX_POINT('',#16121);
#4373=VERTEX_POINT('',#16123);
#4374=VERTEX_POINT('',#16136);
#4375=VERTEX_POINT('',#16138);
#4376=VERTEX_POINT('',#16143);
#4377=VERTEX_POINT('',#16144);
#4378=VERTEX_POINT('',#16146);
#4379=VERTEX_POINT('',#16148);
#4380=VERTEX_POINT('',#16152);
#4381=VERTEX_POINT('',#16154);
#4382=VERTEX_POINT('',#16158);
#4383=VERTEX_POINT('',#16160);
#4384=VERTEX_POINT('',#16168);
#4385=VERTEX_POINT('',#16170);
#4386=VERTEX_POINT('',#16173);
#4387=VERTEX_POINT('',#16175);
#4388=VERTEX_POINT('',#16180);
#4389=VERTEX_POINT('',#16184);
#4390=VERTEX_POINT('',#16191);
#4391=VERTEX_POINT('',#16193);
#4392=VERTEX_POINT('',#16197);
#4393=VERTEX_POINT('',#16199);
#4394=VERTEX_POINT('',#16206);
#4395=VERTEX_POINT('',#16207);
#4396=VERTEX_POINT('',#16211);
#4397=VERTEX_POINT('',#16222);
#4398=VERTEX_POINT('',#16224);
#4399=VERTEX_POINT('',#16226);
#4400=VERTEX_POINT('',#16263);
#4401=VERTEX_POINT('',#16278);
#4402=VERTEX_POINT('',#16280);
#4403=VERTEX_POINT('',#16284);
#4404=VERTEX_POINT('',#16286);
#4405=VERTEX_POINT('',#16293);
#4406=VERTEX_POINT('',#16294);
#4407=VERTEX_POINT('',#16296);
#4408=VERTEX_POINT('',#16298);
#4409=VERTEX_POINT('',#16302);
#4410=VERTEX_POINT('',#16304);
#4411=VERTEX_POINT('',#16308);
#4412=VERTEX_POINT('',#16310);
#4413=VERTEX_POINT('',#16314);
#4414=VERTEX_POINT('',#16320);
#4415=VERTEX_POINT('',#16322);
#4416=VERTEX_POINT('',#16327);
#4417=VERTEX_POINT('',#16333);
#4418=VERTEX_POINT('',#16335);
#4419=VERTEX_POINT('',#16339);
#4420=VERTEX_POINT('',#16341);
#4421=VERTEX_POINT('',#16348);
#4422=VERTEX_POINT('',#16350);
#4423=VERTEX_POINT('',#16354);
#4424=VERTEX_POINT('',#16356);
#4425=VERTEX_POINT('',#16363);
#4426=VERTEX_POINT('',#16366);
#4427=VERTEX_POINT('',#16370);
#4428=VERTEX_POINT('',#16374);
#4429=VERTEX_POINT('',#16378);
#4430=VERTEX_POINT('',#16381);
#4431=VERTEX_POINT('',#16385);
#4432=VERTEX_POINT('',#16389);
#4433=VERTEX_POINT('',#16394);
#4434=VERTEX_POINT('',#16395);
#4435=VERTEX_POINT('',#16397);
#4436=VERTEX_POINT('',#16399);
#4437=VERTEX_POINT('',#16403);
#4438=VERTEX_POINT('',#16405);
#4439=VERTEX_POINT('',#16409);
#4440=VERTEX_POINT('',#16411);
#4441=VERTEX_POINT('',#16415);
#4442=VERTEX_POINT('',#16417);
#4443=VERTEX_POINT('',#16421);
#4444=VERTEX_POINT('',#16423);
#4445=VERTEX_POINT('',#16511);
#4446=VERTEX_POINT('',#16512);
#4447=VERTEX_POINT('',#16514);
#4448=VERTEX_POINT('',#16516);
#4449=VERTEX_POINT('',#16520);
#4450=VERTEX_POINT('',#16522);
#4451=VERTEX_POINT('',#16526);
#4452=VERTEX_POINT('',#16530);
#4453=VERTEX_POINT('',#16536);
#4454=VERTEX_POINT('',#16538);
#4455=VERTEX_POINT('',#16541);
#4456=VERTEX_POINT('',#16543);
#4457=VERTEX_POINT('',#16548);
#4458=VERTEX_POINT('',#16552);
#4459=VERTEX_POINT('',#16559);
#4460=VERTEX_POINT('',#16560);
#4461=VERTEX_POINT('',#16562);
#4462=VERTEX_POINT('',#16564);
#4463=VERTEX_POINT('',#16568);
#4464=VERTEX_POINT('',#16570);
#4465=VERTEX_POINT('',#16574);
#4466=VERTEX_POINT('',#16576);
#4467=VERTEX_POINT('',#16580);
#4468=VERTEX_POINT('',#16586);
#4469=VERTEX_POINT('',#16588);
#4470=VERTEX_POINT('',#16591);
#4471=VERTEX_POINT('',#16599);
#4472=VERTEX_POINT('',#16601);
#4473=VERTEX_POINT('',#16605);
#4474=VERTEX_POINT('',#16607);
#4475=VERTEX_POINT('',#16614);
#4476=VERTEX_POINT('',#16616);
#4477=VERTEX_POINT('',#16620);
#4478=VERTEX_POINT('',#16622);
#4479=VERTEX_POINT('',#16629);
#4480=VERTEX_POINT('',#16630);
#4481=VERTEX_POINT('',#16634);
#4482=VERTEX_POINT('',#16635);
#4483=VERTEX_POINT('',#16642);
#4484=VERTEX_POINT('',#16644);
#4485=VERTEX_POINT('',#16663);
#4486=VERTEX_POINT('',#16665);
#4487=VERTEX_POINT('',#16676);
#4488=VERTEX_POINT('',#16708);
#4489=VERTEX_POINT('',#16711);
#4490=VERTEX_POINT('',#16715);
#4491=VERTEX_POINT('',#16718);
#4492=VERTEX_POINT('',#16725);
#4493=VERTEX_POINT('',#16726);
#4494=VERTEX_POINT('',#16730);
#4495=VERTEX_POINT('',#16731);
#4496=VERTEX_POINT('',#16738);
#4497=VERTEX_POINT('',#16740);
#4498=VERTEX_POINT('',#16759);
#4499=VERTEX_POINT('',#16761);
#4500=VERTEX_POINT('',#16772);
#4501=VERTEX_POINT('',#16804);
#4502=VERTEX_POINT('',#16807);
#4503=VERTEX_POINT('',#16811);
#4504=VERTEX_POINT('',#16814);
#4505=VERTEX_POINT('',#16821);
#4506=VERTEX_POINT('',#16822);
#4507=VERTEX_POINT('',#16824);
#4508=VERTEX_POINT('',#16826);
#4509=VERTEX_POINT('',#16828);
#4510=VERTEX_POINT('',#16830);
#4511=VERTEX_POINT('',#16832);
#4512=VERTEX_POINT('',#16834);
#4513=VERTEX_POINT('',#16838);
#4514=VERTEX_POINT('',#16840);
#4515=VERTEX_POINT('',#16844);
#4516=VERTEX_POINT('',#16848);
#4517=VERTEX_POINT('',#16852);
#4518=VERTEX_POINT('',#16856);
#4519=VERTEX_POINT('',#16858);
#4520=VERTEX_POINT('',#16860);
#4521=VERTEX_POINT('',#16872);
#4522=VERTEX_POINT('',#16875);
#4523=VERTEX_POINT('',#16876);
#4524=VERTEX_POINT('',#16878);
#4525=VERTEX_POINT('',#16880);
#4526=VERTEX_POINT('',#16884);
#4527=VERTEX_POINT('',#16886);
#4528=VERTEX_POINT('',#16890);
#4529=VERTEX_POINT('',#16892);
#4530=VERTEX_POINT('',#16896);
#4531=VERTEX_POINT('',#16898);
#4532=VERTEX_POINT('',#16902);
#4533=VERTEX_POINT('',#16904);
#4534=VERTEX_POINT('',#16912);
#4535=VERTEX_POINT('',#16915);
#4536=EDGE_CURVE('',#3869,#3869,#3457,.T.);
#4537=EDGE_CURVE('',#3869,#3870,#2377,.T.);
#4538=EDGE_CURVE('',#3870,#3870,#3458,.T.);
#4539=EDGE_CURVE('',#3871,#3871,#3459,.T.);
#4540=EDGE_CURVE('',#3871,#3872,#2378,.T.);
#4541=EDGE_CURVE('',#3872,#3872,#3460,.T.);
#4542=EDGE_CURVE('',#3873,#3873,#3461,.T.);
#4543=EDGE_CURVE('',#3873,#3874,#2379,.T.);
#4544=EDGE_CURVE('',#3874,#3874,#3462,.T.);
#4545=EDGE_CURVE('',#3875,#3875,#3463,.T.);
#4546=EDGE_CURVE('',#3875,#3876,#2380,.T.);
#4547=EDGE_CURVE('',#3876,#3876,#3464,.T.);
#4548=EDGE_CURVE('',#3877,#3877,#3465,.T.);
#4549=EDGE_CURVE('',#3877,#3878,#2381,.T.);
#4550=EDGE_CURVE('',#3878,#3878,#3466,.T.);
#4551=EDGE_CURVE('',#3879,#3879,#3467,.T.);
#4552=EDGE_CURVE('',#3879,#3880,#2382,.T.);
#4553=EDGE_CURVE('',#3880,#3880,#3468,.T.);
#4554=EDGE_CURVE('',#3881,#3881,#3469,.T.);
#4555=EDGE_CURVE('',#3881,#3882,#2383,.T.);
#4556=EDGE_CURVE('',#3882,#3882,#3470,.T.);
#4557=EDGE_CURVE('',#3883,#3883,#3471,.T.);
#4558=EDGE_CURVE('',#3883,#3884,#2384,.T.);
#4559=EDGE_CURVE('',#3884,#3884,#3472,.T.);
#4560=EDGE_CURVE('',#3885,#3885,#3473,.T.);
#4561=EDGE_CURVE('',#3885,#3886,#2385,.T.);
#4562=EDGE_CURVE('',#3886,#3886,#3474,.T.);
#4563=EDGE_CURVE('',#3887,#3887,#3475,.T.);
#4564=EDGE_CURVE('',#3887,#3888,#2386,.T.);
#4565=EDGE_CURVE('',#3888,#3888,#3476,.T.);
#4566=EDGE_CURVE('',#3889,#3890,#2387,.T.);
#4567=EDGE_CURVE('',#3890,#3891,#2388,.T.);
#4568=EDGE_CURVE('',#3892,#3891,#2389,.T.);
#4569=EDGE_CURVE('',#3889,#3892,#2390,.T.);
#4570=EDGE_CURVE('',#3893,#3889,#2391,.T.);
#4571=EDGE_CURVE('',#3894,#3892,#2392,.T.);
#4572=EDGE_CURVE('',#3893,#3894,#2393,.T.);
#4573=EDGE_CURVE('',#3895,#3893,#2394,.T.);
#4574=EDGE_CURVE('',#3896,#3894,#2395,.T.);
#4575=EDGE_CURVE('',#3895,#3896,#2396,.T.);
#4576=EDGE_CURVE('',#3890,#3895,#2397,.T.);
#4577=EDGE_CURVE('',#3891,#3896,#2398,.T.);
#4578=EDGE_CURVE('',#3897,#3898,#2399,.T.);
#4579=EDGE_CURVE('',#3898,#3899,#2400,.T.);
#4580=EDGE_CURVE('',#3900,#3899,#2401,.T.);
#4581=EDGE_CURVE('',#3897,#3900,#2402,.T.);
#4582=EDGE_CURVE('',#3901,#3897,#2403,.T.);
#4583=EDGE_CURVE('',#3902,#3900,#2404,.T.);
#4584=EDGE_CURVE('',#3901,#3902,#2405,.T.);
#4585=EDGE_CURVE('',#3903,#3901,#2406,.T.);
#4586=EDGE_CURVE('',#3904,#3902,#2407,.T.);
#4587=EDGE_CURVE('',#3903,#3904,#2408,.T.);
#4588=EDGE_CURVE('',#3898,#3903,#2409,.T.);
#4589=EDGE_CURVE('',#3899,#3904,#2410,.T.);
#4590=EDGE_CURVE('',#3905,#3906,#2411,.T.);
#4591=EDGE_CURVE('',#3906,#3907,#2412,.T.);
#4592=EDGE_CURVE('',#3908,#3907,#2413,.T.);
#4593=EDGE_CURVE('',#3905,#3908,#2414,.T.);
#4594=EDGE_CURVE('',#3909,#3905,#2415,.T.);
#4595=EDGE_CURVE('',#3910,#3908,#2416,.T.);
#4596=EDGE_CURVE('',#3909,#3910,#2417,.T.);
#4597=EDGE_CURVE('',#3911,#3909,#2418,.T.);
#4598=EDGE_CURVE('',#3912,#3910,#2419,.T.);
#4599=EDGE_CURVE('',#3911,#3912,#2420,.T.);
#4600=EDGE_CURVE('',#3906,#3911,#2421,.T.);
#4601=EDGE_CURVE('',#3907,#3912,#2422,.T.);
#4602=EDGE_CURVE('',#3913,#3913,#3477,.T.);
#4603=EDGE_CURVE('',#3913,#3914,#2423,.T.);
#4604=EDGE_CURVE('',#3914,#3914,#3478,.T.);
#4605=EDGE_CURVE('',#3915,#3915,#3479,.T.);
#4606=EDGE_CURVE('',#3915,#3916,#2424,.T.);
#4607=EDGE_CURVE('',#3916,#3916,#3480,.T.);
#4608=EDGE_CURVE('',#3917,#3917,#3481,.T.);
#4609=EDGE_CURVE('',#3917,#3918,#2425,.T.);
#4610=EDGE_CURVE('',#3918,#3918,#3482,.T.);
#4611=EDGE_CURVE('',#3919,#3919,#3483,.T.);
#4612=EDGE_CURVE('',#3919,#3920,#2426,.T.);
#4613=EDGE_CURVE('',#3920,#3920,#3484,.T.);
#4614=EDGE_CURVE('',#3921,#3922,#2427,.T.);
#4615=EDGE_CURVE('',#3923,#3922,#3485,.T.);
#4616=EDGE_CURVE('',#3924,#3923,#2428,.T.);
#4617=EDGE_CURVE('',#3921,#3924,#3486,.T.);
#4618=EDGE_CURVE('',#3925,#3926,#2429,.T.);
#4619=EDGE_CURVE('',#3927,#3926,#3487,.T.);
#4620=EDGE_CURVE('',#3928,#3927,#2430,.T.);
#4621=EDGE_CURVE('',#3925,#3928,#3488,.T.);
#4622=EDGE_CURVE('',#3929,#3930,#2431,.T.);
#4623=EDGE_CURVE('',#3930,#3931,#2432,.T.);
#4624=EDGE_CURVE('',#3931,#3932,#2433,.T.);
#4625=EDGE_CURVE('',#3932,#3929,#2434,.T.);
#4626=EDGE_CURVE('',#3922,#3927,#2435,.T.);
#4627=EDGE_CURVE('',#3926,#3923,#2436,.T.);
#4628=EDGE_CURVE('',#3933,#3934,#3489,.T.);
#4629=EDGE_CURVE('',#3934,#3935,#2437,.T.);
#4630=EDGE_CURVE('',#3935,#3936,#3490,.T.);
#4631=EDGE_CURVE('',#3936,#3933,#2438,.T.);
#4632=EDGE_CURVE('',#3937,#3938,#3491,.T.);
#4633=EDGE_CURVE('',#3938,#3939,#2439,.T.);
#4634=EDGE_CURVE('',#3939,#3940,#3492,.T.);
#4635=EDGE_CURVE('',#3940,#3937,#2440,.T.);
#4636=EDGE_CURVE('',#3941,#3942,#3493,.T.);
#4637=EDGE_CURVE('',#3942,#3943,#2441,.T.);
#4638=EDGE_CURVE('',#3943,#3944,#3494,.T.);
#4639=EDGE_CURVE('',#3944,#3941,#2442,.T.);
#4640=EDGE_CURVE('',#3928,#3921,#2443,.T.);
#4641=EDGE_CURVE('',#3924,#3925,#2444,.T.);
#4642=EDGE_CURVE('',#3945,#3942,#2445,.T.);
#4643=EDGE_CURVE('',#3946,#3941,#2446,.T.);
#4644=EDGE_CURVE('',#3945,#3946,#3495,.T.);
#4645=EDGE_CURVE('',#3947,#3944,#2447,.T.);
#4646=EDGE_CURVE('',#3948,#3943,#2448,.T.);
#4647=EDGE_CURVE('',#3947,#3948,#3496,.T.);
#4648=EDGE_CURVE('',#3948,#3945,#2449,.T.);
#4649=EDGE_CURVE('',#3946,#3947,#2450,.T.);
#4650=EDGE_CURVE('',#3949,#3934,#2451,.T.);
#4651=EDGE_CURVE('',#3950,#3933,#2452,.T.);
#4652=EDGE_CURVE('',#3949,#3950,#3497,.T.);
#4653=EDGE_CURVE('',#3951,#3936,#2453,.T.);
#4654=EDGE_CURVE('',#3952,#3935,#2454,.T.);
#4655=EDGE_CURVE('',#3951,#3952,#3498,.T.);
#4656=EDGE_CURVE('',#3952,#3949,#2455,.T.);
#4657=EDGE_CURVE('',#3950,#3951,#2456,.T.);
#4658=EDGE_CURVE('',#3953,#3938,#2457,.T.);
#4659=EDGE_CURVE('',#3954,#3937,#2458,.T.);
#4660=EDGE_CURVE('',#3953,#3954,#3499,.T.);
#4661=EDGE_CURVE('',#3955,#3940,#2459,.T.);
#4662=EDGE_CURVE('',#3956,#3939,#2460,.T.);
#4663=EDGE_CURVE('',#3955,#3956,#3500,.T.);
#4664=EDGE_CURVE('',#3956,#3953,#2461,.T.);
#4665=EDGE_CURVE('',#3954,#3955,#2462,.T.);
#4666=EDGE_CURVE('',#3957,#3958,#2463,.T.);
#4667=EDGE_CURVE('',#3958,#3929,#2464,.T.);
#4668=EDGE_CURVE('',#3957,#3932,#2465,.T.);
#4669=EDGE_CURVE('',#3959,#3957,#2466,.T.);
#4670=EDGE_CURVE('',#3959,#3931,#2467,.T.);
#4671=EDGE_CURVE('',#3960,#3959,#2468,.T.);
#4672=EDGE_CURVE('',#3960,#3930,#2469,.T.);
#4673=EDGE_CURVE('',#3958,#3960,#2470,.T.);
#4674=EDGE_CURVE('',#3961,#3961,#3501,.T.);
#4675=EDGE_CURVE('',#3961,#3962,#2471,.T.);
#4676=EDGE_CURVE('',#3962,#3962,#3502,.T.);
#4677=EDGE_CURVE('',#3963,#3963,#3503,.T.);
#4678=EDGE_CURVE('',#3963,#3964,#2472,.T.);
#4679=EDGE_CURVE('',#3964,#3964,#3504,.T.);
#4680=EDGE_CURVE('',#3965,#3965,#3505,.T.);
#4681=EDGE_CURVE('',#3965,#3966,#2473,.T.);
#4682=EDGE_CURVE('',#3966,#3966,#3506,.T.);
#4683=EDGE_CURVE('',#3967,#3967,#3507,.T.);
#4684=EDGE_CURVE('',#3967,#3968,#2474,.T.);
#4685=EDGE_CURVE('',#3968,#3968,#3508,.T.);
#4686=EDGE_CURVE('',#3969,#3969,#3509,.T.);
#4687=EDGE_CURVE('',#3969,#3970,#2475,.T.);
#4688=EDGE_CURVE('',#3970,#3970,#3510,.T.);
#4689=EDGE_CURVE('',#3971,#3971,#3511,.T.);
#4690=EDGE_CURVE('',#3971,#3972,#2476,.T.);
#4691=EDGE_CURVE('',#3972,#3972,#3512,.T.);
#4692=EDGE_CURVE('',#3973,#3973,#3513,.T.);
#4693=EDGE_CURVE('',#3973,#3974,#2477,.T.);
#4694=EDGE_CURVE('',#3974,#3974,#3514,.T.);
#4695=EDGE_CURVE('',#3975,#3976,#2478,.T.);
#4696=EDGE_CURVE('',#3977,#3975,#2479,.T.);
#4697=EDGE_CURVE('',#3977,#3978,#2480,.T.);
#4698=EDGE_CURVE('',#3976,#3978,#2481,.T.);
#4699=EDGE_CURVE('',#3979,#3980,#2482,.T.);
#4700=EDGE_CURVE('',#3981,#3979,#2483,.T.);
#4701=EDGE_CURVE('',#3982,#3981,#2484,.T.);
#4702=EDGE_CURVE('',#3980,#3982,#2485,.T.);
#4703=EDGE_CURVE('',#3982,#3983,#2486,.T.);
#4704=EDGE_CURVE('',#3984,#3981,#2487,.T.);
#4705=EDGE_CURVE('',#3983,#3984,#2488,.T.);
#4706=EDGE_CURVE('',#3985,#3977,#2489,.T.);
#4707=EDGE_CURVE('',#3985,#3986,#2490,.T.);
#4708=EDGE_CURVE('',#3978,#3986,#2491,.T.);
#4709=EDGE_CURVE('',#3975,#3987,#2492,.T.);
#4710=EDGE_CURVE('',#3988,#3987,#2493,.T.);
#4711=EDGE_CURVE('',#3980,#3988,#2494,.T.);
#4712=EDGE_CURVE('',#3983,#3985,#2495,.T.);
#4713=EDGE_CURVE('',#3976,#3989,#2496,.T.);
#4714=EDGE_CURVE('',#3987,#3989,#2497,.T.);
#4715=EDGE_CURVE('',#3979,#3990,#2498,.T.);
#4716=EDGE_CURVE('',#3989,#3990,#2499,.T.);
#4717=EDGE_CURVE('',#3986,#3984,#2500,.T.);
#4718=EDGE_CURVE('',#3990,#3988,#2501,.T.);
#4719=EDGE_CURVE('',#3991,#3991,#3515,.T.);
#4720=EDGE_CURVE('',#3991,#3992,#2502,.T.);
#4721=EDGE_CURVE('',#3992,#3992,#3516,.T.);
#4722=EDGE_CURVE('',#3993,#3993,#3517,.T.);
#4723=EDGE_CURVE('',#3993,#3994,#2503,.T.);
#4724=EDGE_CURVE('',#3994,#3994,#3518,.T.);
#4725=EDGE_CURVE('',#3995,#3995,#3519,.T.);
#4726=EDGE_CURVE('',#3995,#3996,#2504,.T.);
#4727=EDGE_CURVE('',#3996,#3996,#3520,.T.);
#4728=EDGE_CURVE('',#3997,#3997,#3521,.T.);
#4729=EDGE_CURVE('',#3997,#3998,#2505,.T.);
#4730=EDGE_CURVE('',#3998,#3998,#3522,.T.);
#4731=EDGE_CURVE('',#3999,#3999,#3523,.T.);
#4732=EDGE_CURVE('',#3999,#4000,#2506,.T.);
#4733=EDGE_CURVE('',#4000,#4000,#3524,.T.);
#4734=EDGE_CURVE('',#4001,#4001,#3525,.T.);
#4735=EDGE_CURVE('',#4001,#4002,#2507,.T.);
#4736=EDGE_CURVE('',#4002,#4002,#3526,.T.);
#4737=EDGE_CURVE('',#4003,#4003,#3527,.T.);
#4738=EDGE_CURVE('',#4003,#4004,#2508,.T.);
#4739=EDGE_CURVE('',#4004,#4004,#3528,.T.);
#4740=EDGE_CURVE('',#4005,#4005,#3529,.T.);
#4741=EDGE_CURVE('',#4005,#4006,#2509,.T.);
#4742=EDGE_CURVE('',#4006,#4006,#3530,.T.);
#4743=EDGE_CURVE('',#4007,#4007,#3531,.T.);
#4744=EDGE_CURVE('',#4007,#4008,#2510,.T.);
#4745=EDGE_CURVE('',#4008,#4008,#3532,.T.);
#4746=EDGE_CURVE('',#4009,#4009,#3533,.T.);
#4747=EDGE_CURVE('',#4009,#4010,#2511,.T.);
#4748=EDGE_CURVE('',#4010,#4010,#3534,.T.);
#4749=EDGE_CURVE('',#4011,#4011,#3535,.T.);
#4750=EDGE_CURVE('',#4011,#4012,#2512,.T.);
#4751=EDGE_CURVE('',#4012,#4012,#3536,.T.);
#4752=EDGE_CURVE('',#4013,#4013,#3537,.T.);
#4753=EDGE_CURVE('',#4013,#4014,#2513,.T.);
#4754=EDGE_CURVE('',#4014,#4014,#3538,.T.);
#4755=EDGE_CURVE('',#4015,#4015,#3539,.T.);
#4756=EDGE_CURVE('',#4016,#4016,#3540,.T.);
#4757=EDGE_CURVE('',#4016,#4015,#2514,.T.);
#4758=EDGE_CURVE('',#4017,#4017,#3541,.T.);
#4759=EDGE_CURVE('',#4017,#4018,#2515,.T.);
#4760=EDGE_CURVE('',#4018,#4018,#3542,.T.);
#4761=EDGE_CURVE('',#4019,#4019,#3543,.T.);
#4762=EDGE_CURVE('',#4019,#4020,#2516,.T.);
#4763=EDGE_CURVE('',#4020,#4020,#3544,.T.);
#4764=EDGE_CURVE('',#4021,#4021,#3545,.T.);
#4765=EDGE_CURVE('',#4021,#4022,#2517,.T.);
#4766=EDGE_CURVE('',#4022,#4022,#3546,.T.);
#4767=EDGE_CURVE('',#4023,#4023,#3547,.T.);
#4768=EDGE_CURVE('',#4023,#4024,#2518,.T.);
#4769=EDGE_CURVE('',#4024,#4024,#3548,.T.);
#4770=EDGE_CURVE('',#4025,#4025,#3549,.T.);
#4771=EDGE_CURVE('',#4025,#4026,#2519,.T.);
#4772=EDGE_CURVE('',#4026,#4026,#3550,.T.);
#4773=EDGE_CURVE('',#4027,#4027,#3551,.T.);
#4774=EDGE_CURVE('',#4027,#4028,#2520,.T.);
#4775=EDGE_CURVE('',#4028,#4028,#3552,.T.);
#4776=EDGE_CURVE('',#4029,#4029,#3553,.T.);
#4777=EDGE_CURVE('',#4029,#4030,#2521,.T.);
#4778=EDGE_CURVE('',#4030,#4030,#3554,.T.);
#4779=EDGE_CURVE('',#4031,#4031,#3555,.T.);
#4780=EDGE_CURVE('',#4031,#4032,#2522,.T.);
#4781=EDGE_CURVE('',#4032,#4032,#3556,.T.);
#4782=EDGE_CURVE('',#4033,#4034,#2523,.T.);
#4783=EDGE_CURVE('',#4035,#4033,#2524,.T.);
#4784=EDGE_CURVE('',#4035,#4036,#2525,.T.);
#4785=EDGE_CURVE('',#4034,#4036,#2526,.T.);
#4786=EDGE_CURVE('',#4037,#4038,#2527,.T.);
#4787=EDGE_CURVE('',#4039,#4037,#2528,.T.);
#4788=EDGE_CURVE('',#4040,#4039,#2529,.T.);
#4789=EDGE_CURVE('',#4038,#4040,#2530,.T.);
#4790=EDGE_CURVE('',#4040,#4041,#2531,.T.);
#4791=EDGE_CURVE('',#4042,#4039,#2532,.T.);
#4792=EDGE_CURVE('',#4041,#4042,#2533,.T.);
#4793=EDGE_CURVE('',#4043,#4035,#2534,.T.);
#4794=EDGE_CURVE('',#4043,#4044,#2535,.T.);
#4795=EDGE_CURVE('',#4036,#4044,#2536,.T.);
#4796=EDGE_CURVE('',#4033,#4045,#2537,.T.);
#4797=EDGE_CURVE('',#4046,#4045,#2538,.T.);
#4798=EDGE_CURVE('',#4038,#4046,#2539,.T.);
#4799=EDGE_CURVE('',#4041,#4043,#2540,.T.);
#4800=EDGE_CURVE('',#4034,#4047,#2541,.T.);
#4801=EDGE_CURVE('',#4045,#4047,#2542,.T.);
#4802=EDGE_CURVE('',#4037,#4048,#2543,.T.);
#4803=EDGE_CURVE('',#4047,#4048,#2544,.T.);
#4804=EDGE_CURVE('',#4044,#4042,#2545,.T.);
#4805=EDGE_CURVE('',#4048,#4046,#2546,.T.);
#4806=EDGE_CURVE('',#4049,#4049,#3557,.T.);
#4807=EDGE_CURVE('',#4049,#4050,#2547,.T.);
#4808=EDGE_CURVE('',#4050,#4050,#3558,.T.);
#4809=EDGE_CURVE('',#4051,#4051,#3559,.T.);
#4810=EDGE_CURVE('',#4051,#4052,#2548,.T.);
#4811=EDGE_CURVE('',#4052,#4052,#3560,.T.);
#4812=EDGE_CURVE('',#4053,#4053,#3561,.T.);
#4813=EDGE_CURVE('',#4053,#4054,#2549,.T.);
#4814=EDGE_CURVE('',#4054,#4054,#3562,.T.);
#4815=EDGE_CURVE('',#4055,#4055,#3563,.T.);
#4816=EDGE_CURVE('',#4055,#4056,#2550,.T.);
#4817=EDGE_CURVE('',#4056,#4056,#3564,.T.);
#4818=EDGE_CURVE('',#4057,#4057,#3565,.T.);
#4819=EDGE_CURVE('',#4057,#4058,#2551,.T.);
#4820=EDGE_CURVE('',#4058,#4058,#3566,.T.);
#4821=EDGE_CURVE('',#4059,#4059,#3567,.T.);
#4822=EDGE_CURVE('',#4059,#4060,#2552,.T.);
#4823=EDGE_CURVE('',#4060,#4060,#3568,.T.);
#4824=EDGE_CURVE('',#4061,#4061,#3569,.T.);
#4825=EDGE_CURVE('',#4061,#4062,#2553,.T.);
#4826=EDGE_CURVE('',#4062,#4062,#3570,.T.);
#4827=EDGE_CURVE('',#4063,#4063,#3571,.T.);
#4828=EDGE_CURVE('',#4063,#4064,#2554,.T.);
#4829=EDGE_CURVE('',#4064,#4064,#3572,.T.);
#4830=EDGE_CURVE('',#4065,#4065,#3573,.T.);
#4831=EDGE_CURVE('',#4065,#4066,#2555,.T.);
#4832=EDGE_CURVE('',#4066,#4066,#3574,.T.);
#4833=EDGE_CURVE('',#4067,#4067,#3575,.T.);
#4834=EDGE_CURVE('',#4067,#4068,#2556,.T.);
#4835=EDGE_CURVE('',#4068,#4068,#3576,.T.);
#4836=EDGE_CURVE('',#4069,#4069,#3577,.T.);
#4837=EDGE_CURVE('',#4069,#4070,#2557,.T.);
#4838=EDGE_CURVE('',#4070,#4070,#3578,.T.);
#4839=EDGE_CURVE('',#4071,#4071,#3579,.T.);
#4840=EDGE_CURVE('',#4071,#4072,#2558,.T.);
#4841=EDGE_CURVE('',#4072,#4072,#3580,.T.);
#4842=EDGE_CURVE('',#4073,#4073,#3581,.T.);
#4843=EDGE_CURVE('',#4074,#4074,#3582,.T.);
#4844=EDGE_CURVE('',#4074,#4073,#2559,.T.);
#4845=EDGE_CURVE('',#4075,#4075,#3583,.T.);
#4846=EDGE_CURVE('',#4075,#4076,#2560,.T.);
#4847=EDGE_CURVE('',#4076,#4076,#3584,.T.);
#4848=EDGE_CURVE('',#4077,#4077,#3585,.T.);
#4849=EDGE_CURVE('',#4077,#4078,#2561,.T.);
#4850=EDGE_CURVE('',#4078,#4078,#3586,.T.);
#4851=EDGE_CURVE('',#4079,#4079,#3587,.T.);
#4852=EDGE_CURVE('',#4079,#4080,#2562,.T.);
#4853=EDGE_CURVE('',#4080,#4080,#3588,.T.);
#4854=EDGE_CURVE('',#4081,#4081,#3589,.T.);
#4855=EDGE_CURVE('',#4081,#4082,#2563,.T.);
#4856=EDGE_CURVE('',#4082,#4082,#3590,.T.);
#4857=EDGE_CURVE('',#4083,#4083,#3591,.T.);
#4858=EDGE_CURVE('',#4083,#4084,#2564,.T.);
#4859=EDGE_CURVE('',#4084,#4084,#3592,.T.);
#4860=EDGE_CURVE('',#4085,#4085,#3593,.T.);
#4861=EDGE_CURVE('',#4085,#4086,#2565,.T.);
#4862=EDGE_CURVE('',#4086,#4086,#3594,.T.);
#4863=EDGE_CURVE('',#4087,#4087,#3595,.T.);
#4864=EDGE_CURVE('',#4087,#4088,#2566,.T.);
#4865=EDGE_CURVE('',#4088,#4088,#3596,.T.);
#4866=EDGE_CURVE('',#4089,#4089,#3597,.T.);
#4867=EDGE_CURVE('',#4089,#4090,#2567,.T.);
#4868=EDGE_CURVE('',#4090,#4090,#3598,.T.);
#4869=EDGE_CURVE('',#4091,#4092,#2568,.T.);
#4870=EDGE_CURVE('',#4093,#4091,#2569,.T.);
#4871=EDGE_CURVE('',#4093,#4094,#2570,.T.);
#4872=EDGE_CURVE('',#4092,#4094,#2571,.T.);
#4873=EDGE_CURVE('',#4095,#4096,#2572,.T.);
#4874=EDGE_CURVE('',#4097,#4095,#2573,.T.);
#4875=EDGE_CURVE('',#4098,#4097,#2574,.T.);
#4876=EDGE_CURVE('',#4096,#4098,#2575,.T.);
#4877=EDGE_CURVE('',#4098,#4099,#2576,.T.);
#4878=EDGE_CURVE('',#4100,#4097,#2577,.T.);
#4879=EDGE_CURVE('',#4099,#4100,#2578,.T.);
#4880=EDGE_CURVE('',#4101,#4093,#2579,.T.);
#4881=EDGE_CURVE('',#4101,#4102,#2580,.T.);
#4882=EDGE_CURVE('',#4094,#4102,#2581,.T.);
#4883=EDGE_CURVE('',#4091,#4103,#2582,.T.);
#4884=EDGE_CURVE('',#4104,#4103,#2583,.T.);
#4885=EDGE_CURVE('',#4096,#4104,#2584,.T.);
#4886=EDGE_CURVE('',#4099,#4101,#2585,.T.);
#4887=EDGE_CURVE('',#4092,#4105,#2586,.T.);
#4888=EDGE_CURVE('',#4103,#4105,#2587,.T.);
#4889=EDGE_CURVE('',#4095,#4106,#2588,.T.);
#4890=EDGE_CURVE('',#4105,#4106,#2589,.T.);
#4891=EDGE_CURVE('',#4102,#4100,#2590,.T.);
#4892=EDGE_CURVE('',#4106,#4104,#2591,.T.);
#4893=EDGE_CURVE('',#4107,#4107,#3599,.T.);
#4894=EDGE_CURVE('',#4107,#4108,#2592,.T.);
#4895=EDGE_CURVE('',#4108,#4108,#3600,.T.);
#4896=EDGE_CURVE('',#4109,#4109,#3601,.T.);
#4897=EDGE_CURVE('',#4109,#4110,#2593,.T.);
#4898=EDGE_CURVE('',#4110,#4110,#3602,.T.);
#4899=EDGE_CURVE('',#4111,#4111,#3603,.T.);
#4900=EDGE_CURVE('',#4111,#4112,#2594,.T.);
#4901=EDGE_CURVE('',#4112,#4112,#3604,.T.);
#4902=EDGE_CURVE('',#4113,#4113,#3605,.T.);
#4903=EDGE_CURVE('',#4113,#4114,#2595,.T.);
#4904=EDGE_CURVE('',#4114,#4114,#3606,.T.);
#4905=EDGE_CURVE('',#4115,#4115,#3607,.T.);
#4906=EDGE_CURVE('',#4115,#4116,#2596,.T.);
#4907=EDGE_CURVE('',#4116,#4116,#3608,.T.);
#4908=EDGE_CURVE('',#4117,#4117,#3609,.T.);
#4909=EDGE_CURVE('',#4117,#4118,#2597,.T.);
#4910=EDGE_CURVE('',#4118,#4118,#3610,.T.);
#4911=EDGE_CURVE('',#4119,#4119,#3611,.T.);
#4912=EDGE_CURVE('',#4119,#4120,#2598,.T.);
#4913=EDGE_CURVE('',#4120,#4120,#3612,.T.);
#4914=EDGE_CURVE('',#4121,#4121,#3613,.T.);
#4915=EDGE_CURVE('',#4121,#4122,#2599,.T.);
#4916=EDGE_CURVE('',#4122,#4122,#3614,.T.);
#4917=EDGE_CURVE('',#4123,#4123,#3615,.T.);
#4918=EDGE_CURVE('',#4123,#4124,#2600,.T.);
#4919=EDGE_CURVE('',#4124,#4124,#3616,.T.);
#4920=EDGE_CURVE('',#4125,#4125,#3617,.T.);
#4921=EDGE_CURVE('',#4125,#4126,#2601,.T.);
#4922=EDGE_CURVE('',#4126,#4126,#3618,.T.);
#4923=EDGE_CURVE('',#4127,#4127,#3619,.T.);
#4924=EDGE_CURVE('',#4127,#4128,#2602,.T.);
#4925=EDGE_CURVE('',#4128,#4128,#3620,.T.);
#4926=EDGE_CURVE('',#4129,#4129,#3621,.T.);
#4927=EDGE_CURVE('',#4129,#4130,#2603,.T.);
#4928=EDGE_CURVE('',#4130,#4130,#3622,.T.);
#4929=EDGE_CURVE('',#4131,#4131,#3623,.T.);
#4930=EDGE_CURVE('',#4132,#4132,#3624,.T.);
#4931=EDGE_CURVE('',#4132,#4131,#2604,.T.);
#4932=EDGE_CURVE('',#4133,#4133,#3625,.T.);
#4933=EDGE_CURVE('',#4133,#4134,#2605,.T.);
#4934=EDGE_CURVE('',#4134,#4134,#3626,.T.);
#4935=EDGE_CURVE('',#4135,#4135,#3627,.T.);
#4936=EDGE_CURVE('',#4135,#4136,#2606,.T.);
#4937=EDGE_CURVE('',#4136,#4136,#3628,.T.);
#4938=EDGE_CURVE('',#4137,#4137,#3629,.T.);
#4939=EDGE_CURVE('',#4137,#4138,#2607,.T.);
#4940=EDGE_CURVE('',#4138,#4138,#3630,.T.);
#4941=EDGE_CURVE('',#4139,#4139,#3631,.T.);
#4942=EDGE_CURVE('',#4139,#4140,#2608,.T.);
#4943=EDGE_CURVE('',#4140,#4140,#3632,.T.);
#4944=EDGE_CURVE('',#4141,#4141,#3633,.T.);
#4945=EDGE_CURVE('',#4141,#4142,#2609,.T.);
#4946=EDGE_CURVE('',#4142,#4142,#3634,.T.);
#4947=EDGE_CURVE('',#4143,#4143,#3635,.T.);
#4948=EDGE_CURVE('',#4143,#4144,#2610,.T.);
#4949=EDGE_CURVE('',#4144,#4144,#3636,.T.);
#4950=EDGE_CURVE('',#4145,#4145,#3637,.T.);
#4951=EDGE_CURVE('',#4145,#4146,#2611,.T.);
#4952=EDGE_CURVE('',#4146,#4146,#3638,.T.);
#4953=EDGE_CURVE('',#4147,#4147,#3639,.T.);
#4954=EDGE_CURVE('',#4147,#4148,#2612,.T.);
#4955=EDGE_CURVE('',#4148,#4148,#3640,.T.);
#4956=EDGE_CURVE('',#4149,#4150,#2613,.T.);
#4957=EDGE_CURVE('',#4151,#4149,#2614,.T.);
#4958=EDGE_CURVE('',#4151,#4152,#2615,.T.);
#4959=EDGE_CURVE('',#4150,#4152,#2616,.T.);
#4960=EDGE_CURVE('',#4153,#4154,#2617,.T.);
#4961=EDGE_CURVE('',#4155,#4153,#2618,.T.);
#4962=EDGE_CURVE('',#4156,#4155,#2619,.T.);
#4963=EDGE_CURVE('',#4154,#4156,#2620,.T.);
#4964=EDGE_CURVE('',#4156,#4157,#2621,.T.);
#4965=EDGE_CURVE('',#4158,#4155,#2622,.T.);
#4966=EDGE_CURVE('',#4157,#4158,#2623,.T.);
#4967=EDGE_CURVE('',#4159,#4151,#2624,.T.);
#4968=EDGE_CURVE('',#4159,#4160,#2625,.T.);
#4969=EDGE_CURVE('',#4152,#4160,#2626,.T.);
#4970=EDGE_CURVE('',#4149,#4161,#2627,.T.);
#4971=EDGE_CURVE('',#4162,#4161,#2628,.T.);
#4972=EDGE_CURVE('',#4154,#4162,#2629,.T.);
#4973=EDGE_CURVE('',#4157,#4159,#2630,.T.);
#4974=EDGE_CURVE('',#4150,#4163,#2631,.T.);
#4975=EDGE_CURVE('',#4161,#4163,#2632,.T.);
#4976=EDGE_CURVE('',#4153,#4164,#2633,.T.);
#4977=EDGE_CURVE('',#4163,#4164,#2634,.T.);
#4978=EDGE_CURVE('',#4160,#4158,#2635,.T.);
#4979=EDGE_CURVE('',#4164,#4162,#2636,.T.);
#4980=EDGE_CURVE('',#4165,#4165,#3641,.T.);
#4981=EDGE_CURVE('',#4165,#4166,#2637,.T.);
#4982=EDGE_CURVE('',#4166,#4166,#3642,.T.);
#4983=EDGE_CURVE('',#4167,#4167,#3643,.T.);
#4984=EDGE_CURVE('',#4167,#4168,#2638,.T.);
#4985=EDGE_CURVE('',#4168,#4168,#3644,.T.);
#4986=EDGE_CURVE('',#4169,#4169,#3645,.T.);
#4987=EDGE_CURVE('',#4169,#4170,#2639,.T.);
#4988=EDGE_CURVE('',#4170,#4170,#3646,.T.);
#4989=EDGE_CURVE('',#4171,#4171,#3647,.T.);
#4990=EDGE_CURVE('',#4171,#4172,#2640,.T.);
#4991=EDGE_CURVE('',#4172,#4172,#3648,.T.);
#4992=EDGE_CURVE('',#4173,#4173,#3649,.T.);
#4993=EDGE_CURVE('',#4173,#4174,#2641,.T.);
#4994=EDGE_CURVE('',#4174,#4174,#3650,.T.);
#4995=EDGE_CURVE('',#4175,#4175,#3651,.T.);
#4996=EDGE_CURVE('',#4175,#4176,#2642,.T.);
#4997=EDGE_CURVE('',#4176,#4176,#3652,.T.);
#4998=EDGE_CURVE('',#4177,#4177,#3653,.T.);
#4999=EDGE_CURVE('',#4177,#4178,#2643,.T.);
#5000=EDGE_CURVE('',#4178,#4178,#3654,.T.);
#5001=EDGE_CURVE('',#4179,#4179,#3655,.T.);
#5002=EDGE_CURVE('',#4179,#4180,#2644,.T.);
#5003=EDGE_CURVE('',#4180,#4180,#3656,.T.);
#5004=EDGE_CURVE('',#4181,#4181,#3657,.T.);
#5005=EDGE_CURVE('',#4181,#4182,#2645,.T.);
#5006=EDGE_CURVE('',#4182,#4182,#3658,.T.);
#5007=EDGE_CURVE('',#4183,#4183,#3659,.T.);
#5008=EDGE_CURVE('',#4183,#4184,#2646,.T.);
#5009=EDGE_CURVE('',#4184,#4184,#3660,.T.);
#5010=EDGE_CURVE('',#4185,#4185,#3661,.T.);
#5011=EDGE_CURVE('',#4185,#4186,#2647,.T.);
#5012=EDGE_CURVE('',#4186,#4186,#3662,.T.);
#5013=EDGE_CURVE('',#4187,#4187,#3663,.T.);
#5014=EDGE_CURVE('',#4187,#4188,#2648,.T.);
#5015=EDGE_CURVE('',#4188,#4188,#3664,.T.);
#5016=EDGE_CURVE('',#4189,#4189,#3665,.T.);
#5017=EDGE_CURVE('',#4190,#4190,#3666,.T.);
#5018=EDGE_CURVE('',#4190,#4189,#2649,.T.);
#5019=EDGE_CURVE('',#4191,#4191,#3667,.T.);
#5020=EDGE_CURVE('',#4191,#4192,#2650,.T.);
#5021=EDGE_CURVE('',#4192,#4192,#3668,.T.);
#5022=EDGE_CURVE('',#4193,#4193,#3669,.T.);
#5023=EDGE_CURVE('',#4193,#4194,#2651,.T.);
#5024=EDGE_CURVE('',#4194,#4194,#3670,.T.);
#5025=EDGE_CURVE('',#4195,#4195,#3671,.T.);
#5026=EDGE_CURVE('',#4195,#4196,#2652,.T.);
#5027=EDGE_CURVE('',#4196,#4196,#3672,.T.);
#5028=EDGE_CURVE('',#4197,#4197,#3673,.T.);
#5029=EDGE_CURVE('',#4197,#4198,#2653,.T.);
#5030=EDGE_CURVE('',#4198,#4198,#3674,.T.);
#5031=EDGE_CURVE('',#4199,#4199,#3675,.T.);
#5032=EDGE_CURVE('',#4200,#4200,#3676,.T.);
#5033=EDGE_CURVE('',#4200,#4199,#2654,.T.);
#5034=EDGE_CURVE('',#4201,#4201,#3677,.T.);
#5035=EDGE_CURVE('',#4201,#4202,#2655,.T.);
#5036=EDGE_CURVE('',#4202,#4202,#3678,.T.);
#5037=EDGE_CURVE('',#4203,#4203,#3679,.T.);
#5038=EDGE_CURVE('',#4204,#4204,#3680,.T.);
#5039=EDGE_CURVE('',#4204,#4203,#2656,.T.);
#5040=EDGE_CURVE('',#4205,#4206,#2657,.T.);
#5041=EDGE_CURVE('',#4206,#4207,#2658,.T.);
#5042=EDGE_CURVE('',#4208,#4207,#2659,.T.);
#5043=EDGE_CURVE('',#4205,#4208,#2660,.T.);
#5044=EDGE_CURVE('',#4209,#4205,#2661,.T.);
#5045=EDGE_CURVE('',#4210,#4208,#2662,.T.);
#5046=EDGE_CURVE('',#4209,#4210,#2663,.T.);
#5047=EDGE_CURVE('',#4211,#4209,#2664,.T.);
#5048=EDGE_CURVE('',#4212,#4210,#2665,.T.);
#5049=EDGE_CURVE('',#4211,#4212,#2666,.T.);
#5050=EDGE_CURVE('',#4206,#4211,#2667,.T.);
#5051=EDGE_CURVE('',#4207,#4212,#2668,.T.);
#5052=EDGE_CURVE('',#4213,#4213,#3681,.T.);
#5053=EDGE_CURVE('',#4213,#4214,#2669,.T.);
#5054=EDGE_CURVE('',#4214,#4214,#3682,.T.);
#5055=EDGE_CURVE('',#4215,#4215,#3683,.T.);
#5056=EDGE_CURVE('',#4215,#4216,#2670,.T.);
#5057=EDGE_CURVE('',#4216,#4216,#3684,.T.);
#5058=EDGE_CURVE('',#4217,#4217,#3685,.T.);
#5059=EDGE_CURVE('',#4217,#4218,#481,.T.);
#5060=EDGE_CURVE('',#4218,#4218,#3686,.T.);
#5061=EDGE_CURVE('',#4219,#4219,#3687,.T.);
#5062=EDGE_CURVE('',#4219,#4220,#2671,.T.);
#5063=EDGE_CURVE('',#4220,#4220,#3688,.T.);
#5064=EDGE_CURVE('',#4221,#4221,#3689,.T.);
#5065=EDGE_CURVE('',#4221,#4222,#2672,.T.);
#5066=EDGE_CURVE('',#4222,#4222,#3690,.T.);
#5067=EDGE_CURVE('',#4223,#4223,#3691,.T.);
#5068=EDGE_CURVE('',#4223,#4224,#482,.T.);
#5069=EDGE_CURVE('',#4224,#4224,#3692,.T.);
#5070=EDGE_CURVE('',#4225,#4225,#3693,.T.);
#5071=EDGE_CURVE('',#4226,#4226,#3694,.T.);
#5072=EDGE_CURVE('',#4226,#4225,#2673,.T.);
#5073=EDGE_CURVE('',#4227,#4227,#3695,.T.);
#5074=EDGE_CURVE('',#4227,#4226,#2674,.T.);
#5075=EDGE_CURVE('',#4228,#4228,#3696,.T.);
#5076=EDGE_CURVE('',#4228,#4227,#2675,.T.);
#5077=EDGE_CURVE('',#4229,#4229,#3697,.T.);
#5078=EDGE_CURVE('',#4230,#4230,#3698,.F.);
#5079=EDGE_CURVE('',#4230,#4229,#2676,.T.);
#5080=EDGE_CURVE('',#4231,#4231,#3699,.F.);
#5081=EDGE_CURVE('',#4231,#4230,#2677,.T.);
#5082=EDGE_CURVE('',#4232,#4232,#3700,.T.);
#5083=EDGE_CURVE('',#4232,#4231,#2678,.T.);
#5084=EDGE_CURVE('',#4233,#4234,#2679,.T.);
#5085=EDGE_CURVE('',#4234,#4235,#2680,.T.);
#5086=EDGE_CURVE('',#4235,#4236,#2681,.T.);
#5087=EDGE_CURVE('',#4233,#4236,#2682,.T.);
#5088=EDGE_CURVE('',#4234,#4237,#2683,.T.);
#5089=EDGE_CURVE('',#4237,#4238,#2684,.T.);
#5090=EDGE_CURVE('',#4238,#4235,#2685,.T.);
#5091=EDGE_CURVE('',#4237,#4239,#2686,.T.);
#5092=EDGE_CURVE('',#4239,#4240,#2687,.T.);
#5093=EDGE_CURVE('',#4240,#4238,#2688,.T.);
#5094=EDGE_CURVE('',#4239,#4241,#2689,.T.);
#5095=EDGE_CURVE('',#4241,#4242,#2690,.T.);
#5096=EDGE_CURVE('',#4242,#4240,#2691,.T.);
#5097=EDGE_CURVE('',#4241,#4243,#2692,.T.);
#5098=EDGE_CURVE('',#4243,#4244,#2693,.T.);
#5099=EDGE_CURVE('',#4244,#4242,#2694,.T.);
#5100=EDGE_CURVE('',#4243,#4233,#2695,.T.);
#5101=EDGE_CURVE('',#4236,#4244,#2696,.T.);
#5102=EDGE_CURVE('',#4245,#4246,#3701,.T.);
#5103=EDGE_CURVE('',#4246,#4245,#3702,.T.);
#5104=EDGE_CURVE('',#4246,#4247,#3703,.T.);
#5105=EDGE_CURVE('',#4248,#4247,#3704,.T.);
#5106=EDGE_CURVE('',#4247,#4248,#3705,.T.);
#5107=EDGE_CURVE('',#4248,#4249,#2697,.T.);
#5108=EDGE_CURVE('',#4249,#4249,#3706,.T.);
#5109=EDGE_CURVE('',#4250,#4250,#3707,.T.);
#5110=EDGE_CURVE('',#4250,#4251,#2698,.T.);
#5111=EDGE_CURVE('',#4251,#4251,#3708,.T.);
#5112=EDGE_CURVE('',#4251,#4252,#2699,.T.);
#5113=EDGE_CURVE('',#4252,#4252,#3709,.T.);
#5114=EDGE_CURVE('',#4253,#4253,#3710,.T.);
#5115=EDGE_CURVE('',#4253,#4245,#2700,.T.);
#5116=EDGE_CURVE('',#4254,#4254,#3711,.T.);
#5117=EDGE_CURVE('',#4254,#4250,#2701,.T.);
#5118=EDGE_CURVE('',#4255,#4256,#3712,.T.);
#5119=EDGE_CURVE('',#4256,#4255,#3713,.T.);
#5120=EDGE_CURVE('',#4256,#4257,#3714,.T.);
#5121=EDGE_CURVE('',#4258,#4257,#3715,.T.);
#5122=EDGE_CURVE('',#4257,#4258,#3716,.T.);
#5123=EDGE_CURVE('',#4259,#4259,#3717,.T.);
#5124=EDGE_CURVE('',#4259,#4258,#2702,.T.);
#5125=EDGE_CURVE('',#4260,#4260,#3718,.T.);
#5126=EDGE_CURVE('',#4261,#4261,#3719,.T.);
#5127=EDGE_CURVE('',#4262,#4262,#3720,.T.);
#5128=EDGE_CURVE('',#4262,#4260,#2703,.T.);
#5129=EDGE_CURVE('',#4263,#4263,#3721,.T.);
#5130=EDGE_CURVE('',#4263,#4262,#2704,.T.);
#5131=EDGE_CURVE('',#4264,#4264,#3722,.T.);
#5132=EDGE_CURVE('',#4264,#4263,#2705,.T.);
#5133=EDGE_CURVE('',#4255,#4261,#2706,.T.);
#5134=EDGE_CURVE('',#4265,#4266,#3723,.T.);
#5135=EDGE_CURVE('',#4267,#4268,#3724,.T.);
#5136=EDGE_CURVE('',#4269,#4270,#3725,.T.);
#5137=EDGE_CURVE('',#4271,#4272,#3726,.T.);
#5138=EDGE_CURVE('',#4273,#4274,#3727,.T.);
#5139=EDGE_CURVE('',#4275,#4276,#3728,.T.);
#5140=EDGE_CURVE('',#4277,#4278,#3729,.T.);
#5141=EDGE_CURVE('',#4279,#4280,#483,.T.);
#5142=EDGE_CURVE('',#4281,#4279,#3730,.T.);
#5143=EDGE_CURVE('',#4282,#4281,#484,.T.);
#5144=EDGE_CURVE('',#4280,#4282,#3731,.T.);
#5145=EDGE_CURVE('',#4283,#4281,#3732,.T.);
#5146=EDGE_CURVE('',#4283,#4284,#485,.T.);
#5147=EDGE_CURVE('',#4285,#4284,#3733,.T.);
#5148=EDGE_CURVE('',#4285,#4286,#486,.T.);
#5149=EDGE_CURVE('',#4287,#4286,#3734,.T.);
#5150=EDGE_CURVE('',#4287,#4288,#2707,.T.);
#5151=EDGE_CURVE('',#4288,#4288,#3735,.T.);
#5152=EDGE_CURVE('',#4289,#4287,#3736,.T.);
#5153=EDGE_CURVE('',#4289,#4290,#487,.T.);
#5154=EDGE_CURVE('',#4291,#4290,#3737,.T.);
#5155=EDGE_CURVE('',#4291,#4292,#488,.T.);
#5156=EDGE_CURVE('',#4293,#4292,#3738,.T.);
#5157=EDGE_CURVE('',#4293,#4294,#489,.T.);
#5158=EDGE_CURVE('',#4295,#4294,#3739,.T.);
#5159=EDGE_CURVE('',#4295,#4296,#490,.T.);
#5160=EDGE_CURVE('',#4282,#4296,#3740,.T.);
#5161=EDGE_CURVE('',#4279,#4297,#3741,.T.);
#5162=EDGE_CURVE('',#4297,#4283,#3742,.T.);
#5163=EDGE_CURVE('',#4298,#4297,#491,.T.);
#5164=EDGE_CURVE('',#4284,#4298,#3743,.T.);
#5165=EDGE_CURVE('',#4298,#4299,#3744,.T.);
#5166=EDGE_CURVE('',#4299,#4285,#3745,.T.);
#5167=EDGE_CURVE('',#4300,#4299,#492,.T.);
#5168=EDGE_CURVE('',#4286,#4300,#3746,.T.);
#5169=EDGE_CURVE('',#4300,#4301,#3747,.T.);
#5170=EDGE_CURVE('',#4301,#4302,#3748,.T.);
#5171=EDGE_CURVE('',#4302,#4289,#3749,.T.);
#5172=EDGE_CURVE('',#4303,#4302,#493,.T.);
#5173=EDGE_CURVE('',#4290,#4303,#3750,.T.);
#5174=EDGE_CURVE('',#4303,#4304,#3751,.T.);
#5175=EDGE_CURVE('',#4304,#4291,#3752,.T.);
#5176=EDGE_CURVE('',#4305,#4304,#494,.T.);
#5177=EDGE_CURVE('',#4292,#4305,#3753,.T.);
#5178=EDGE_CURVE('',#4305,#4306,#3754,.T.);
#5179=EDGE_CURVE('',#4306,#4293,#3755,.T.);
#5180=EDGE_CURVE('',#4307,#4306,#495,.T.);
#5181=EDGE_CURVE('',#4294,#4307,#3756,.T.);
#5182=EDGE_CURVE('',#4308,#4308,#3757,.T.);
#5183=EDGE_CURVE('',#4308,#4301,#2708,.T.);
#5184=EDGE_CURVE('',#4309,#4280,#3758,.T.);
#5185=EDGE_CURVE('',#4309,#4310,#496,.T.);
#5186=EDGE_CURVE('',#4307,#4310,#3759,.T.);
#5187=EDGE_CURVE('',#4296,#4309,#3760,.T.);
#5188=EDGE_CURVE('',#4310,#4295,#3761,.T.);
#5189=EDGE_CURVE('',#4311,#4311,#3762,.T.);
#5190=EDGE_CURVE('',#4312,#4312,#3763,.T.);
#5191=EDGE_CURVE('',#4313,#4313,#3764,.T.);
#5192=EDGE_CURVE('',#4313,#4311,#2709,.T.);
#5193=EDGE_CURVE('',#4314,#4314,#3765,.T.);
#5194=EDGE_CURVE('',#4314,#4312,#2710,.T.);
#5195=EDGE_CURVE('',#4315,#4315,#3766,.T.);
#5196=EDGE_CURVE('',#4316,#4316,#3767,.T.);
#5197=EDGE_CURVE('',#4317,#4317,#3768,.T.);
#5198=EDGE_CURVE('',#4317,#4315,#2711,.T.);
#5199=EDGE_CURVE('',#4318,#4318,#3769,.T.);
#5200=EDGE_CURVE('',#4318,#4316,#2712,.T.);
#5201=EDGE_CURVE('',#4319,#4320,#2713,.T.);
#5202=EDGE_CURVE('',#4320,#4321,#2714,.T.);
#5203=EDGE_CURVE('',#4321,#4322,#2715,.T.);
#5204=EDGE_CURVE('',#4319,#4322,#2716,.T.);
#5205=EDGE_CURVE('',#4320,#4323,#2717,.T.);
#5206=EDGE_CURVE('',#4323,#4324,#2718,.T.);
#5207=EDGE_CURVE('',#4324,#4321,#2719,.T.);
#5208=EDGE_CURVE('',#4323,#4325,#2720,.T.);
#5209=EDGE_CURVE('',#4325,#4326,#2721,.T.);
#5210=EDGE_CURVE('',#4326,#4324,#2722,.T.);
#5211=EDGE_CURVE('',#4325,#4327,#2723,.T.);
#5212=EDGE_CURVE('',#4327,#4328,#2724,.T.);
#5213=EDGE_CURVE('',#4328,#4326,#2725,.T.);
#5214=EDGE_CURVE('',#4327,#4329,#2726,.T.);
#5215=EDGE_CURVE('',#4329,#4330,#2727,.T.);
#5216=EDGE_CURVE('',#4330,#4328,#2728,.T.);
#5217=EDGE_CURVE('',#4329,#4319,#2729,.T.);
#5218=EDGE_CURVE('',#4322,#4330,#2730,.T.);
#5219=EDGE_CURVE('',#4331,#4331,#3770,.T.);
#5220=EDGE_CURVE('',#4332,#4332,#3771,.T.);
#5221=EDGE_CURVE('',#4333,#4333,#3772,.T.);
#5222=EDGE_CURVE('',#4333,#4332,#2731,.T.);
#5223=EDGE_CURVE('',#4334,#4334,#3773,.T.);
#5224=EDGE_CURVE('',#4334,#4333,#2732,.T.);
#5225=EDGE_CURVE('',#4335,#4335,#3774,.T.);
#5226=EDGE_CURVE('',#4335,#4334,#2733,.T.);
#5227=EDGE_CURVE('',#4336,#4336,#3775,.T.);
#5228=EDGE_CURVE('',#4337,#4337,#3776,.F.);
#5229=EDGE_CURVE('',#4337,#4336,#2734,.T.);
#5230=EDGE_CURVE('',#4331,#4337,#2735,.T.);
#5231=EDGE_CURVE('',#4338,#4338,#3777,.T.);
#5232=EDGE_CURVE('',#4339,#4339,#3778,.T.);
#5233=EDGE_CURVE('',#4339,#4338,#2736,.T.);
#5234=EDGE_CURVE('',#4340,#4340,#3779,.T.);
#5235=EDGE_CURVE('',#4340,#4339,#2737,.T.);
#5236=EDGE_CURVE('',#4341,#4341,#3780,.T.);
#5237=EDGE_CURVE('',#4341,#4340,#2738,.T.);
#5238=EDGE_CURVE('',#4342,#4342,#3781,.T.);
#5239=EDGE_CURVE('',#4343,#4343,#3782,.F.);
#5240=EDGE_CURVE('',#4343,#4342,#2739,.T.);
#5241=EDGE_CURVE('',#4344,#4344,#3783,.F.);
#5242=EDGE_CURVE('',#4344,#4343,#2740,.T.);
#5243=EDGE_CURVE('',#4345,#4345,#3784,.T.);
#5244=EDGE_CURVE('',#4345,#4344,#2741,.T.);
#5245=EDGE_CURVE('',#4346,#4347,#2742,.T.);
#5246=EDGE_CURVE('',#4347,#4348,#2743,.T.);
#5247=EDGE_CURVE('',#4348,#4349,#2744,.T.);
#5248=EDGE_CURVE('',#4346,#4349,#2745,.T.);
#5249=EDGE_CURVE('',#4347,#4350,#2746,.T.);
#5250=EDGE_CURVE('',#4350,#4351,#2747,.T.);
#5251=EDGE_CURVE('',#4351,#4348,#2748,.T.);
#5252=EDGE_CURVE('',#4350,#4352,#2749,.T.);
#5253=EDGE_CURVE('',#4352,#4353,#2750,.T.);
#5254=EDGE_CURVE('',#4353,#4351,#2751,.T.);
#5255=EDGE_CURVE('',#4352,#4354,#2752,.T.);
#5256=EDGE_CURVE('',#4354,#4355,#2753,.T.);
#5257=EDGE_CURVE('',#4355,#4353,#2754,.T.);
#5258=EDGE_CURVE('',#4354,#4356,#2755,.T.);
#5259=EDGE_CURVE('',#4356,#4357,#2756,.T.);
#5260=EDGE_CURVE('',#4357,#4355,#2757,.T.);
#5261=EDGE_CURVE('',#4356,#4346,#2758,.T.);
#5262=EDGE_CURVE('',#4349,#4357,#2759,.T.);
#5263=EDGE_CURVE('',#4358,#4359,#11,.T.);
#5264=EDGE_CURVE('',#4360,#4358,#12,.T.);
#5265=EDGE_CURVE('',#4360,#4361,#2760,.T.);
#5266=EDGE_CURVE('',#4361,#4361,#3785,.T.);
#5267=EDGE_CURVE('',#4362,#4360,#13,.T.);
#5268=EDGE_CURVE('',#4363,#4362,#14,.T.);
#5269=EDGE_CURVE('',#4364,#4363,#15,.T.);
#5270=EDGE_CURVE('',#4359,#4364,#16,.T.);
#5271=EDGE_CURVE('',#4365,#4365,#3786,.T.);
#5272=EDGE_CURVE('',#4365,#4366,#2761,.T.);
#5273=EDGE_CURVE('',#4367,#4366,#17,.T.);
#5274=EDGE_CURVE('',#4368,#4367,#18,.T.);
#5275=EDGE_CURVE('',#4369,#4368,#19,.T.);
#5276=EDGE_CURVE('',#4370,#4369,#20,.T.);
#5277=EDGE_CURVE('',#4371,#4370,#21,.T.);
#5278=EDGE_CURVE('',#4366,#4371,#22,.T.);
#5279=EDGE_CURVE('',#4362,#4371,#2762,.T.);
#5280=EDGE_CURVE('',#4363,#4370,#2763,.T.);
#5281=EDGE_CURVE('',#4360,#4366,#2764,.T.);
#5282=EDGE_CURVE('',#4358,#4367,#2765,.T.);
#5283=EDGE_CURVE('',#4372,#4372,#3787,.F.);
#5284=EDGE_CURVE('',#4372,#4373,#2766,.T.);
#5285=EDGE_CURVE('',#4373,#4373,#3788,.F.);
#5286=EDGE_CURVE('',#4359,#4368,#2767,.T.);
#5287=EDGE_CURVE('',#4364,#4369,#2768,.T.);
#5288=EDGE_CURVE('',#4374,#4374,#3789,.T.);
#5289=EDGE_CURVE('',#4374,#4375,#2769,.T.);
#5290=EDGE_CURVE('',#4375,#4375,#3790,.T.);
#5291=EDGE_CURVE('',#4376,#4377,#2770,.T.);
#5292=EDGE_CURVE('',#4376,#4378,#2771,.T.);
#5293=EDGE_CURVE('',#4379,#4378,#2772,.T.);
#5294=EDGE_CURVE('',#4379,#4377,#2773,.T.);
#5295=EDGE_CURVE('',#4377,#4380,#3791,.T.);
#5296=EDGE_CURVE('',#4381,#4379,#2774,.T.);
#5297=EDGE_CURVE('',#4380,#4381,#2775,.T.);
#5298=EDGE_CURVE('',#4380,#4382,#2776,.T.);
#5299=EDGE_CURVE('',#4381,#4383,#2777,.T.);
#5300=EDGE_CURVE('',#4383,#4382,#2778,.T.);
#5301=EDGE_CURVE('',#4378,#4383,#2779,.T.);
#5302=EDGE_CURVE('',#4382,#4376,#3792,.T.);
#5303=EDGE_CURVE('',#4384,#4384,#3793,.T.);
#5304=EDGE_CURVE('',#4385,#4385,#3794,.T.);
#5305=EDGE_CURVE('',#4386,#4386,#3795,.T.);
#5306=EDGE_CURVE('',#4387,#4387,#3796,.T.);
#5307=EDGE_CURVE('',#4384,#4386,#2780,.T.);
#5308=EDGE_CURVE('',#4387,#4388,#2781,.T.);
#5309=EDGE_CURVE('',#4388,#4388,#3797,.T.);
#5310=EDGE_CURVE('',#4389,#4389,#3798,.T.);
#5311=EDGE_CURVE('',#4389,#4385,#2782,.T.);
#5312=EDGE_CURVE('',#4390,#4390,#3799,.T.);
#5313=EDGE_CURVE('',#4390,#4391,#2783,.T.);
#5314=EDGE_CURVE('',#4391,#4391,#3800,.T.);
#5315=EDGE_CURVE('',#4392,#4392,#3801,.T.);
#5316=EDGE_CURVE('',#4392,#4393,#2784,.T.);
#5317=EDGE_CURVE('',#4393,#4393,#3802,.T.);
#5318=EDGE_CURVE('',#4394,#4395,#2785,.T.);
#5319=EDGE_CURVE('',#4394,#4395,#3803,.T.);
#5320=EDGE_CURVE('',#4396,#4394,#497,.T.);
#5321=EDGE_CURVE('',#4397,#4396,#3804,.T.);
#5322=EDGE_CURVE('',#4397,#4398,#2786,.T.);
#5323=EDGE_CURVE('',#4399,#4398,#498,.T.);
#5324=EDGE_CURVE('',#4398,#4399,#499,.T.);
#5325=EDGE_CURVE('',#4400,#4397,#3805,.T.);
#5326=EDGE_CURVE('',#4395,#4400,#500,.T.);
#5327=EDGE_CURVE('',#4400,#4396,#2787,.T.);
#5328=EDGE_CURVE('',#4401,#4401,#3806,.T.);
#5329=EDGE_CURVE('',#4401,#4402,#2788,.T.);
#5330=EDGE_CURVE('',#4402,#4402,#3807,.T.);
#5331=EDGE_CURVE('',#4403,#4403,#3808,.T.);
#5332=EDGE_CURVE('',#4403,#4404,#2789,.T.);
#5333=EDGE_CURVE('',#4404,#4404,#3809,.T.);
#5334=EDGE_CURVE('',#4405,#4406,#2790,.T.);
#5335=EDGE_CURVE('',#4405,#4407,#2791,.T.);
#5336=EDGE_CURVE('',#4408,#4407,#2792,.T.);
#5337=EDGE_CURVE('',#4406,#4408,#2793,.T.);
#5338=EDGE_CURVE('',#4409,#4405,#2794,.T.);
#5339=EDGE_CURVE('',#4409,#4410,#2795,.T.);
#5340=EDGE_CURVE('',#4407,#4410,#2796,.T.);
#5341=EDGE_CURVE('',#4411,#4409,#2797,.T.);
#5342=EDGE_CURVE('',#4412,#4411,#2798,.T.);
#5343=EDGE_CURVE('',#4410,#4412,#2799,.T.);
#5344=EDGE_CURVE('',#4413,#4413,#3810,.T.);
#5345=EDGE_CURVE('',#4412,#4408,#3811,.T.);
#5346=EDGE_CURVE('',#4411,#4406,#3812,.T.);
#5347=EDGE_CURVE('',#4414,#4414,#3813,.T.);
#5348=EDGE_CURVE('',#4415,#4415,#3814,.T.);
#5349=EDGE_CURVE('',#4413,#4414,#2800,.T.);
#5350=EDGE_CURVE('',#4415,#4416,#2801,.T.);
#5351=EDGE_CURVE('',#4416,#4416,#3815,.T.);
#5352=EDGE_CURVE('',#4417,#4417,#3816,.T.);
#5353=EDGE_CURVE('',#4417,#4418,#2802,.T.);
#5354=EDGE_CURVE('',#4418,#4418,#3817,.T.);
#5355=EDGE_CURVE('',#4419,#4419,#3818,.T.);
#5356=EDGE_CURVE('',#4419,#4420,#2803,.T.);
#5357=EDGE_CURVE('',#4420,#4420,#3819,.T.);
#5358=EDGE_CURVE('',#4421,#4421,#3820,.T.);
#5359=EDGE_CURVE('',#4421,#4422,#2804,.T.);
#5360=EDGE_CURVE('',#4422,#4422,#3821,.T.);
#5361=EDGE_CURVE('',#4423,#4423,#3822,.T.);
#5362=EDGE_CURVE('',#4423,#4424,#2805,.T.);
#5363=EDGE_CURVE('',#4424,#4424,#3823,.T.);
#5364=EDGE_CURVE('',#4425,#4425,#3824,.T.);
#5365=EDGE_CURVE('',#4426,#4426,#3825,.T.);
#5366=EDGE_CURVE('',#4426,#4425,#2806,.T.);
#5367=EDGE_CURVE('',#4427,#4427,#3826,.T.);
#5368=EDGE_CURVE('',#4427,#4426,#2807,.T.);
#5369=EDGE_CURVE('',#4428,#4428,#3827,.T.);
#5370=EDGE_CURVE('',#4428,#4427,#2808,.T.);
#5371=EDGE_CURVE('',#4429,#4429,#3828,.T.);
#5372=EDGE_CURVE('',#4430,#4430,#3829,.F.);
#5373=EDGE_CURVE('',#4430,#4429,#2809,.T.);
#5374=EDGE_CURVE('',#4431,#4431,#3830,.F.);
#5375=EDGE_CURVE('',#4431,#4430,#2810,.T.);
#5376=EDGE_CURVE('',#4432,#4432,#3831,.T.);
#5377=EDGE_CURVE('',#4432,#4431,#2811,.T.);
#5378=EDGE_CURVE('',#4433,#4434,#2812,.T.);
#5379=EDGE_CURVE('',#4434,#4435,#2813,.T.);
#5380=EDGE_CURVE('',#4435,#4436,#2814,.T.);
#5381=EDGE_CURVE('',#4433,#4436,#2815,.T.);
#5382=EDGE_CURVE('',#4434,#4437,#2816,.T.);
#5383=EDGE_CURVE('',#4437,#4438,#2817,.T.);
#5384=EDGE_CURVE('',#4438,#4435,#2818,.T.);
#5385=EDGE_CURVE('',#4437,#4439,#2819,.T.);
#5386=EDGE_CURVE('',#4439,#4440,#2820,.T.);
#5387=EDGE_CURVE('',#4440,#4438,#2821,.T.);
#5388=EDGE_CURVE('',#4439,#4441,#2822,.T.);
#5389=EDGE_CURVE('',#4441,#4442,#2823,.T.);
#5390=EDGE_CURVE('',#4442,#4440,#2824,.T.);
#5391=EDGE_CURVE('',#4441,#4443,#2825,.T.);
#5392=EDGE_CURVE('',#4443,#4444,#2826,.T.);
#5393=EDGE_CURVE('',#4444,#4442,#2827,.T.);
#5394=EDGE_CURVE('',#4443,#4433,#2828,.T.);
#5395=EDGE_CURVE('',#4436,#4444,#2829,.T.);
#5396=EDGE_CURVE('',#4445,#4446,#2830,.T.);
#5397=EDGE_CURVE('',#4445,#4447,#2831,.T.);
#5398=EDGE_CURVE('',#4448,#4447,#2832,.T.);
#5399=EDGE_CURVE('',#4446,#4448,#2833,.T.);
#5400=EDGE_CURVE('',#4446,#4449,#3832,.T.);
#5401=EDGE_CURVE('',#4448,#4450,#2834,.T.);
#5402=EDGE_CURVE('',#4450,#4449,#2835,.T.);
#5403=EDGE_CURVE('',#4447,#4451,#2836,.T.);
#5404=EDGE_CURVE('',#4450,#4451,#2837,.T.);
#5405=EDGE_CURVE('',#4449,#4452,#2838,.T.);
#5406=EDGE_CURVE('',#4451,#4452,#2839,.T.);
#5407=EDGE_CURVE('',#4452,#4445,#3833,.T.);
#5408=EDGE_CURVE('',#4453,#4453,#3834,.T.);
#5409=EDGE_CURVE('',#4454,#4454,#3835,.T.);
#5410=EDGE_CURVE('',#4455,#4455,#3836,.T.);
#5411=EDGE_CURVE('',#4456,#4456,#3837,.T.);
#5412=EDGE_CURVE('',#4453,#4455,#2840,.T.);
#5413=EDGE_CURVE('',#4456,#4457,#2841,.T.);
#5414=EDGE_CURVE('',#4457,#4457,#3838,.T.);
#5415=EDGE_CURVE('',#4458,#4458,#3839,.T.);
#5416=EDGE_CURVE('',#4458,#4454,#2842,.T.);
#5417=EDGE_CURVE('',#4459,#4460,#2843,.T.);
#5418=EDGE_CURVE('',#4459,#4461,#2844,.T.);
#5419=EDGE_CURVE('',#4462,#4461,#2845,.T.);
#5420=EDGE_CURVE('',#4460,#4462,#2846,.T.);
#5421=EDGE_CURVE('',#4463,#4459,#2847,.T.);
#5422=EDGE_CURVE('',#4463,#4464,#2848,.T.);
#5423=EDGE_CURVE('',#4461,#4464,#2849,.T.);
#5424=EDGE_CURVE('',#4465,#4463,#2850,.T.);
#5425=EDGE_CURVE('',#4466,#4465,#2851,.T.);
#5426=EDGE_CURVE('',#4464,#4466,#2852,.T.);
#5427=EDGE_CURVE('',#4467,#4467,#3840,.T.);
#5428=EDGE_CURVE('',#4466,#4462,#3841,.T.);
#5429=EDGE_CURVE('',#4465,#4460,#3842,.T.);
#5430=EDGE_CURVE('',#4468,#4468,#3843,.T.);
#5431=EDGE_CURVE('',#4469,#4469,#3844,.T.);
#5432=EDGE_CURVE('',#4468,#4470,#2853,.T.);
#5433=EDGE_CURVE('',#4470,#4470,#3845,.T.);
#5434=EDGE_CURVE('',#4467,#4469,#2854,.T.);
#5435=EDGE_CURVE('',#4471,#4471,#3846,.T.);
#5436=EDGE_CURVE('',#4471,#4472,#2855,.T.);
#5437=EDGE_CURVE('',#4472,#4472,#3847,.T.);
#5438=EDGE_CURVE('',#4473,#4473,#3848,.T.);
#5439=EDGE_CURVE('',#4473,#4474,#2856,.T.);
#5440=EDGE_CURVE('',#4474,#4474,#3849,.T.);
#5441=EDGE_CURVE('',#4475,#4475,#3850,.T.);
#5442=EDGE_CURVE('',#4475,#4476,#2857,.T.);
#5443=EDGE_CURVE('',#4476,#4476,#3851,.T.);
#5444=EDGE_CURVE('',#4477,#4477,#3852,.T.);
#5445=EDGE_CURVE('',#4477,#4478,#2858,.T.);
#5446=EDGE_CURVE('',#4478,#4478,#3853,.T.);
#5447=EDGE_CURVE('',#4479,#4480,#2859,.T.);
#5448=EDGE_CURVE('',#4479,#4480,#3854,.T.);
#5449=EDGE_CURVE('',#4481,#4482,#501,.T.);
#5450=EDGE_CURVE('',#4483,#4481,#3855,.T.);
#5451=EDGE_CURVE('',#4484,#4483,#502,.T.);
#5452=EDGE_CURVE('',#4480,#4484,#503,.T.);
#5453=EDGE_CURVE('',#4482,#4479,#504,.T.);
#5454=EDGE_CURVE('',#4482,#4485,#2860,.T.);
#5455=EDGE_CURVE('',#4486,#4485,#505,.T.);
#5456=EDGE_CURVE('',#4487,#4486,#506,.T.);
#5457=EDGE_CURVE('',#4485,#4487,#507,.T.);
#5458=EDGE_CURVE('',#4483,#4481,#2861,.T.);
#5459=EDGE_CURVE('',#4488,#4488,#3856,.T.);
#5460=EDGE_CURVE('',#4488,#4484,#2862,.T.);
#5461=EDGE_CURVE('',#4482,#4489,#2863,.T.);
#5462=EDGE_CURVE('',#4489,#4489,#3857,.T.);
#5463=EDGE_CURVE('',#4490,#4490,#3858,.T.);
#5464=EDGE_CURVE('',#4490,#4487,#2864,.T.);
#5465=EDGE_CURVE('',#4485,#4491,#2865,.T.);
#5466=EDGE_CURVE('',#4491,#4491,#3859,.T.);
#5467=EDGE_CURVE('',#4492,#4493,#2866,.T.);
#5468=EDGE_CURVE('',#4492,#4493,#3860,.T.);
#5469=EDGE_CURVE('',#4494,#4495,#508,.T.);
#5470=EDGE_CURVE('',#4496,#4494,#3861,.T.);
#5471=EDGE_CURVE('',#4497,#4496,#509,.T.);
#5472=EDGE_CURVE('',#4493,#4497,#510,.T.);
#5473=EDGE_CURVE('',#4495,#4492,#511,.T.);
#5474=EDGE_CURVE('',#4495,#4498,#2867,.T.);
#5475=EDGE_CURVE('',#4499,#4498,#512,.T.);
#5476=EDGE_CURVE('',#4500,#4499,#513,.T.);
#5477=EDGE_CURVE('',#4498,#4500,#514,.T.);
#5478=EDGE_CURVE('',#4496,#4494,#2868,.T.);
#5479=EDGE_CURVE('',#4501,#4501,#3862,.T.);
#5480=EDGE_CURVE('',#4501,#4497,#2869,.T.);
#5481=EDGE_CURVE('',#4495,#4502,#2870,.T.);
#5482=EDGE_CURVE('',#4502,#4502,#3863,.T.);
#5483=EDGE_CURVE('',#4503,#4503,#3864,.T.);
#5484=EDGE_CURVE('',#4503,#4500,#2871,.T.);
#5485=EDGE_CURVE('',#4498,#4504,#2872,.T.);
#5486=EDGE_CURVE('',#4504,#4504,#3865,.T.);
#5487=EDGE_CURVE('',#4505,#4506,#2873,.T.);
#5488=EDGE_CURVE('',#4507,#4505,#2874,.T.);
#5489=EDGE_CURVE('',#4508,#4507,#2875,.T.);
#5490=EDGE_CURVE('',#4509,#4508,#2876,.T.);
#5491=EDGE_CURVE('',#4510,#4509,#2877,.T.);
#5492=EDGE_CURVE('',#4511,#4510,#2878,.T.);
#5493=EDGE_CURVE('',#4512,#4511,#2879,.T.);
#5494=EDGE_CURVE('',#4506,#4512,#2880,.T.);
#5495=EDGE_CURVE('',#4509,#4513,#2881,.T.);
#5496=EDGE_CURVE('',#4513,#4514,#2882,.T.);
#5497=EDGE_CURVE('',#4514,#4510,#2883,.T.);
#5498=EDGE_CURVE('',#4515,#4508,#2884,.T.);
#5499=EDGE_CURVE('',#4515,#4513,#2885,.T.);
#5500=EDGE_CURVE('',#4507,#4516,#2886,.T.);
#5501=EDGE_CURVE('',#4516,#4515,#2887,.T.);
#5502=EDGE_CURVE('',#4517,#4505,#2888,.T.);
#5503=EDGE_CURVE('',#4517,#4516,#2889,.T.);
#5504=EDGE_CURVE('',#4518,#4517,#2890,.T.);
#5505=EDGE_CURVE('',#4519,#4518,#2891,.T.);
#5506=EDGE_CURVE('',#4520,#4519,#2892,.T.);
#5507=EDGE_CURVE('',#4514,#4520,#2893,.T.);
#5508=EDGE_CURVE('',#4506,#4518,#2894,.T.);
#5509=EDGE_CURVE('',#4519,#4512,#2895,.T.);
#5510=EDGE_CURVE('',#4511,#4520,#2896,.T.);
#5511=EDGE_CURVE('',#4521,#4521,#3866,.T.);
#5512=EDGE_CURVE('',#4522,#4523,#2897,.T.);
#5513=EDGE_CURVE('',#4522,#4524,#2898,.T.);
#5514=EDGE_CURVE('',#4524,#4525,#2899,.T.);
#5515=EDGE_CURVE('',#4523,#4525,#2900,.T.);
#5516=EDGE_CURVE('',#4526,#4522,#2901,.T.);
#5517=EDGE_CURVE('',#4526,#4527,#2902,.T.);
#5518=EDGE_CURVE('',#4527,#4524,#2903,.T.);
#5519=EDGE_CURVE('',#4528,#4526,#2904,.T.);
#5520=EDGE_CURVE('',#4528,#4529,#2905,.T.);
#5521=EDGE_CURVE('',#4529,#4527,#2906,.T.);
#5522=EDGE_CURVE('',#4530,#4528,#2907,.T.);
#5523=EDGE_CURVE('',#4530,#4531,#2908,.T.);
#5524=EDGE_CURVE('',#4531,#4529,#2909,.T.);
#5525=EDGE_CURVE('',#4532,#4530,#2910,.T.);
#5526=EDGE_CURVE('',#4532,#4533,#2911,.T.);
#5527=EDGE_CURVE('',#4533,#4531,#2912,.T.);
#5528=EDGE_CURVE('',#4523,#4532,#2913,.T.);
#5529=EDGE_CURVE('',#4525,#4533,#2914,.T.);
#5530=EDGE_CURVE('',#4534,#4534,#3867,.T.);
#5531=EDGE_CURVE('',#4535,#4535,#3868,.T.);
#5532=EDGE_CURVE('',#4535,#4534,#2915,.T.);
#5533=EDGE_CURVE('',#4521,#4535,#2916,.T.);
#5534=ORIENTED_EDGE('',*,*,#4536,.F.);
#5535=ORIENTED_EDGE('',*,*,#4537,.T.);
#5536=ORIENTED_EDGE('',*,*,#4538,.F.);
#5537=ORIENTED_EDGE('',*,*,#4537,.F.);
#5538=ORIENTED_EDGE('',*,*,#4539,.F.);
#5539=ORIENTED_EDGE('',*,*,#4540,.T.);
#5540=ORIENTED_EDGE('',*,*,#4541,.F.);
#5541=ORIENTED_EDGE('',*,*,#4540,.F.);
#5542=ORIENTED_EDGE('',*,*,#4542,.F.);
#5543=ORIENTED_EDGE('',*,*,#4543,.T.);
#5544=ORIENTED_EDGE('',*,*,#4544,.F.);
#5545=ORIENTED_EDGE('',*,*,#4543,.F.);
#5546=ORIENTED_EDGE('',*,*,#4545,.F.);
#5547=ORIENTED_EDGE('',*,*,#4546,.T.);
#5548=ORIENTED_EDGE('',*,*,#4547,.F.);
#5549=ORIENTED_EDGE('',*,*,#4546,.F.);
#5550=ORIENTED_EDGE('',*,*,#4548,.F.);
#5551=ORIENTED_EDGE('',*,*,#4549,.T.);
#5552=ORIENTED_EDGE('',*,*,#4550,.F.);
#5553=ORIENTED_EDGE('',*,*,#4549,.F.);
#5554=ORIENTED_EDGE('',*,*,#4551,.F.);
#5555=ORIENTED_EDGE('',*,*,#4552,.T.);
#5556=ORIENTED_EDGE('',*,*,#4553,.F.);
#5557=ORIENTED_EDGE('',*,*,#4552,.F.);
#5558=ORIENTED_EDGE('',*,*,#4554,.F.);
#5559=ORIENTED_EDGE('',*,*,#4555,.T.);
#5560=ORIENTED_EDGE('',*,*,#4556,.F.);
#5561=ORIENTED_EDGE('',*,*,#4555,.F.);
#5562=ORIENTED_EDGE('',*,*,#4557,.F.);
#5563=ORIENTED_EDGE('',*,*,#4558,.T.);
#5564=ORIENTED_EDGE('',*,*,#4559,.F.);
#5565=ORIENTED_EDGE('',*,*,#4558,.F.);
#5566=ORIENTED_EDGE('',*,*,#4560,.F.);
#5567=ORIENTED_EDGE('',*,*,#4561,.T.);
#5568=ORIENTED_EDGE('',*,*,#4562,.F.);
#5569=ORIENTED_EDGE('',*,*,#4561,.F.);
#5570=ORIENTED_EDGE('',*,*,#4563,.F.);
#5571=ORIENTED_EDGE('',*,*,#4564,.T.);
#5572=ORIENTED_EDGE('',*,*,#4565,.F.);
#5573=ORIENTED_EDGE('',*,*,#4564,.F.);
#5574=ORIENTED_EDGE('',*,*,#4566,.T.);
#5575=ORIENTED_EDGE('',*,*,#4567,.T.);
#5576=ORIENTED_EDGE('',*,*,#4568,.F.);
#5577=ORIENTED_EDGE('',*,*,#4569,.F.);
#5578=ORIENTED_EDGE('',*,*,#4570,.T.);
#5579=ORIENTED_EDGE('',*,*,#4569,.T.);
#5580=ORIENTED_EDGE('',*,*,#4571,.F.);
#5581=ORIENTED_EDGE('',*,*,#4572,.F.);
#5582=ORIENTED_EDGE('',*,*,#4573,.T.);
#5583=ORIENTED_EDGE('',*,*,#4572,.T.);
#5584=ORIENTED_EDGE('',*,*,#4574,.F.);
#5585=ORIENTED_EDGE('',*,*,#4575,.F.);
#5586=ORIENTED_EDGE('',*,*,#4576,.T.);
#5587=ORIENTED_EDGE('',*,*,#4575,.T.);
#5588=ORIENTED_EDGE('',*,*,#4577,.F.);
#5589=ORIENTED_EDGE('',*,*,#4567,.F.);
#5590=ORIENTED_EDGE('',*,*,#4577,.T.);
#5591=ORIENTED_EDGE('',*,*,#4574,.T.);
#5592=ORIENTED_EDGE('',*,*,#4571,.T.);
#5593=ORIENTED_EDGE('',*,*,#4568,.T.);
#5594=ORIENTED_EDGE('',*,*,#4541,.T.);
#5595=ORIENTED_EDGE('',*,*,#4565,.T.);
#5596=ORIENTED_EDGE('',*,*,#4562,.T.);
#5597=ORIENTED_EDGE('',*,*,#4559,.T.);
#5598=ORIENTED_EDGE('',*,*,#4556,.T.);
#5599=ORIENTED_EDGE('',*,*,#4553,.T.);
#5600=ORIENTED_EDGE('',*,*,#4550,.T.);
#5601=ORIENTED_EDGE('',*,*,#4547,.T.);
#5602=ORIENTED_EDGE('',*,*,#4544,.T.);
#5603=ORIENTED_EDGE('',*,*,#4538,.T.);
#5604=ORIENTED_EDGE('',*,*,#4576,.F.);
#5605=ORIENTED_EDGE('',*,*,#4566,.F.);
#5606=ORIENTED_EDGE('',*,*,#4570,.F.);
#5607=ORIENTED_EDGE('',*,*,#4573,.F.);
#5608=ORIENTED_EDGE('',*,*,#4539,.T.);
#5609=ORIENTED_EDGE('',*,*,#4563,.T.);
#5610=ORIENTED_EDGE('',*,*,#4560,.T.);
#5611=ORIENTED_EDGE('',*,*,#4557,.T.);
#5612=ORIENTED_EDGE('',*,*,#4554,.T.);
#5613=ORIENTED_EDGE('',*,*,#4551,.T.);
#5614=ORIENTED_EDGE('',*,*,#4548,.T.);
#5615=ORIENTED_EDGE('',*,*,#4545,.T.);
#5616=ORIENTED_EDGE('',*,*,#4542,.T.);
#5617=ORIENTED_EDGE('',*,*,#4536,.T.);
#5618=ORIENTED_EDGE('',*,*,#4578,.T.);
#5619=ORIENTED_EDGE('',*,*,#4579,.T.);
#5620=ORIENTED_EDGE('',*,*,#4580,.F.);
#5621=ORIENTED_EDGE('',*,*,#4581,.F.);
#5622=ORIENTED_EDGE('',*,*,#4582,.T.);
#5623=ORIENTED_EDGE('',*,*,#4581,.T.);
#5624=ORIENTED_EDGE('',*,*,#4583,.F.);
#5625=ORIENTED_EDGE('',*,*,#4584,.F.);
#5626=ORIENTED_EDGE('',*,*,#4585,.T.);
#5627=ORIENTED_EDGE('',*,*,#4584,.T.);
#5628=ORIENTED_EDGE('',*,*,#4586,.F.);
#5629=ORIENTED_EDGE('',*,*,#4587,.F.);
#5630=ORIENTED_EDGE('',*,*,#4588,.T.);
#5631=ORIENTED_EDGE('',*,*,#4587,.T.);
#5632=ORIENTED_EDGE('',*,*,#4589,.F.);
#5633=ORIENTED_EDGE('',*,*,#4579,.F.);
#5634=ORIENTED_EDGE('',*,*,#4589,.T.);
#5635=ORIENTED_EDGE('',*,*,#4586,.T.);
#5636=ORIENTED_EDGE('',*,*,#4583,.T.);
#5637=ORIENTED_EDGE('',*,*,#4580,.T.);
#5638=ORIENTED_EDGE('',*,*,#4588,.F.);
#5639=ORIENTED_EDGE('',*,*,#4578,.F.);
#5640=ORIENTED_EDGE('',*,*,#4582,.F.);
#5641=ORIENTED_EDGE('',*,*,#4585,.F.);
#5642=ORIENTED_EDGE('',*,*,#4590,.T.);
#5643=ORIENTED_EDGE('',*,*,#4591,.T.);
#5644=ORIENTED_EDGE('',*,*,#4592,.F.);
#5645=ORIENTED_EDGE('',*,*,#4593,.F.);
#5646=ORIENTED_EDGE('',*,*,#4594,.T.);
#5647=ORIENTED_EDGE('',*,*,#4593,.T.);
#5648=ORIENTED_EDGE('',*,*,#4595,.F.);
#5649=ORIENTED_EDGE('',*,*,#4596,.F.);
#5650=ORIENTED_EDGE('',*,*,#4597,.T.);
#5651=ORIENTED_EDGE('',*,*,#4596,.T.);
#5652=ORIENTED_EDGE('',*,*,#4598,.F.);
#5653=ORIENTED_EDGE('',*,*,#4599,.F.);
#5654=ORIENTED_EDGE('',*,*,#4600,.T.);
#5655=ORIENTED_EDGE('',*,*,#4599,.T.);
#5656=ORIENTED_EDGE('',*,*,#4601,.F.);
#5657=ORIENTED_EDGE('',*,*,#4591,.F.);
#5658=ORIENTED_EDGE('',*,*,#4601,.T.);
#5659=ORIENTED_EDGE('',*,*,#4598,.T.);
#5660=ORIENTED_EDGE('',*,*,#4595,.T.);
#5661=ORIENTED_EDGE('',*,*,#4592,.T.);
#5662=ORIENTED_EDGE('',*,*,#4600,.F.);
#5663=ORIENTED_EDGE('',*,*,#4590,.F.);
#5664=ORIENTED_EDGE('',*,*,#4594,.F.);
#5665=ORIENTED_EDGE('',*,*,#4597,.F.);
#5666=ORIENTED_EDGE('',*,*,#4602,.F.);
#5667=ORIENTED_EDGE('',*,*,#4603,.T.);
#5668=ORIENTED_EDGE('',*,*,#4604,.F.);
#5669=ORIENTED_EDGE('',*,*,#4603,.F.);
#5670=ORIENTED_EDGE('',*,*,#4605,.F.);
#5671=ORIENTED_EDGE('',*,*,#4606,.T.);
#5672=ORIENTED_EDGE('',*,*,#4607,.F.);
#5673=ORIENTED_EDGE('',*,*,#4606,.F.);
#5674=ORIENTED_EDGE('',*,*,#4608,.F.);
#5675=ORIENTED_EDGE('',*,*,#4609,.T.);
#5676=ORIENTED_EDGE('',*,*,#4610,.F.);
#5677=ORIENTED_EDGE('',*,*,#4609,.F.);
#5678=ORIENTED_EDGE('',*,*,#4611,.F.);
#5679=ORIENTED_EDGE('',*,*,#4612,.T.);
#5680=ORIENTED_EDGE('',*,*,#4613,.F.);
#5681=ORIENTED_EDGE('',*,*,#4612,.F.);
#5682=ORIENTED_EDGE('',*,*,#4614,.T.);
#5683=ORIENTED_EDGE('',*,*,#4615,.F.);
#5684=ORIENTED_EDGE('',*,*,#4616,.F.);
#5685=ORIENTED_EDGE('',*,*,#4617,.F.);
#5686=ORIENTED_EDGE('',*,*,#4618,.T.);
#5687=ORIENTED_EDGE('',*,*,#4619,.F.);
#5688=ORIENTED_EDGE('',*,*,#4620,.F.);
#5689=ORIENTED_EDGE('',*,*,#4621,.F.);
#5690=ORIENTED_EDGE('',*,*,#4622,.T.);
#5691=ORIENTED_EDGE('',*,*,#4623,.T.);
#5692=ORIENTED_EDGE('',*,*,#4624,.T.);
#5693=ORIENTED_EDGE('',*,*,#4625,.T.);
#5694=ORIENTED_EDGE('',*,*,#4615,.T.);
#5695=ORIENTED_EDGE('',*,*,#4626,.T.);
#5696=ORIENTED_EDGE('',*,*,#4619,.T.);
#5697=ORIENTED_EDGE('',*,*,#4627,.T.);
#5698=ORIENTED_EDGE('',*,*,#4628,.T.);
#5699=ORIENTED_EDGE('',*,*,#4629,.T.);
#5700=ORIENTED_EDGE('',*,*,#4630,.T.);
#5701=ORIENTED_EDGE('',*,*,#4631,.T.);
#5702=ORIENTED_EDGE('',*,*,#4632,.T.);
#5703=ORIENTED_EDGE('',*,*,#4633,.T.);
#5704=ORIENTED_EDGE('',*,*,#4634,.T.);
#5705=ORIENTED_EDGE('',*,*,#4635,.T.);
#5706=ORIENTED_EDGE('',*,*,#4636,.T.);
#5707=ORIENTED_EDGE('',*,*,#4637,.T.);
#5708=ORIENTED_EDGE('',*,*,#4638,.T.);
#5709=ORIENTED_EDGE('',*,*,#4639,.T.);
#5710=ORIENTED_EDGE('',*,*,#4613,.T.);
#5711=ORIENTED_EDGE('',*,*,#4610,.T.);
#5712=ORIENTED_EDGE('',*,*,#4607,.T.);
#5713=ORIENTED_EDGE('',*,*,#4604,.T.);
#5714=ORIENTED_EDGE('',*,*,#4626,.F.);
#5715=ORIENTED_EDGE('',*,*,#4614,.F.);
#5716=ORIENTED_EDGE('',*,*,#4640,.F.);
#5717=ORIENTED_EDGE('',*,*,#4620,.T.);
#5718=ORIENTED_EDGE('',*,*,#4627,.F.);
#5719=ORIENTED_EDGE('',*,*,#4618,.F.);
#5720=ORIENTED_EDGE('',*,*,#4641,.F.);
#5721=ORIENTED_EDGE('',*,*,#4616,.T.);
#5722=ORIENTED_EDGE('',*,*,#4642,.T.);
#5723=ORIENTED_EDGE('',*,*,#4636,.F.);
#5724=ORIENTED_EDGE('',*,*,#4643,.F.);
#5725=ORIENTED_EDGE('',*,*,#4644,.F.);
#5726=ORIENTED_EDGE('',*,*,#4645,.T.);
#5727=ORIENTED_EDGE('',*,*,#4638,.F.);
#5728=ORIENTED_EDGE('',*,*,#4646,.F.);
#5729=ORIENTED_EDGE('',*,*,#4647,.F.);
#5730=ORIENTED_EDGE('',*,*,#4637,.F.);
#5731=ORIENTED_EDGE('',*,*,#4642,.F.);
#5732=ORIENTED_EDGE('',*,*,#4648,.F.);
#5733=ORIENTED_EDGE('',*,*,#4646,.T.);
#5734=ORIENTED_EDGE('',*,*,#4639,.F.);
#5735=ORIENTED_EDGE('',*,*,#4645,.F.);
#5736=ORIENTED_EDGE('',*,*,#4649,.F.);
#5737=ORIENTED_EDGE('',*,*,#4643,.T.);
#5738=ORIENTED_EDGE('',*,*,#4650,.T.);
#5739=ORIENTED_EDGE('',*,*,#4628,.F.);
#5740=ORIENTED_EDGE('',*,*,#4651,.F.);
#5741=ORIENTED_EDGE('',*,*,#4652,.F.);
#5742=ORIENTED_EDGE('',*,*,#4653,.T.);
#5743=ORIENTED_EDGE('',*,*,#4630,.F.);
#5744=ORIENTED_EDGE('',*,*,#4654,.F.);
#5745=ORIENTED_EDGE('',*,*,#4655,.F.);
#5746=ORIENTED_EDGE('',*,*,#4629,.F.);
#5747=ORIENTED_EDGE('',*,*,#4650,.F.);
#5748=ORIENTED_EDGE('',*,*,#4656,.F.);
#5749=ORIENTED_EDGE('',*,*,#4654,.T.);
#5750=ORIENTED_EDGE('',*,*,#4631,.F.);
#5751=ORIENTED_EDGE('',*,*,#4653,.F.);
#5752=ORIENTED_EDGE('',*,*,#4657,.F.);
#5753=ORIENTED_EDGE('',*,*,#4651,.T.);
#5754=ORIENTED_EDGE('',*,*,#4658,.T.);
#5755=ORIENTED_EDGE('',*,*,#4632,.F.);
#5756=ORIENTED_EDGE('',*,*,#4659,.F.);
#5757=ORIENTED_EDGE('',*,*,#4660,.F.);
#5758=ORIENTED_EDGE('',*,*,#4661,.T.);
#5759=ORIENTED_EDGE('',*,*,#4634,.F.);
#5760=ORIENTED_EDGE('',*,*,#4662,.F.);
#5761=ORIENTED_EDGE('',*,*,#4663,.F.);
#5762=ORIENTED_EDGE('',*,*,#4633,.F.);
#5763=ORIENTED_EDGE('',*,*,#4658,.F.);
#5764=ORIENTED_EDGE('',*,*,#4664,.F.);
#5765=ORIENTED_EDGE('',*,*,#4662,.T.);
#5766=ORIENTED_EDGE('',*,*,#4635,.F.);
#5767=ORIENTED_EDGE('',*,*,#4661,.F.);
#5768=ORIENTED_EDGE('',*,*,#4665,.F.);
#5769=ORIENTED_EDGE('',*,*,#4659,.T.);
#5770=ORIENTED_EDGE('',*,*,#4666,.T.);
#5771=ORIENTED_EDGE('',*,*,#4667,.T.);
#5772=ORIENTED_EDGE('',*,*,#4625,.F.);
#5773=ORIENTED_EDGE('',*,*,#4668,.F.);
#5774=ORIENTED_EDGE('',*,*,#4669,.T.);
#5775=ORIENTED_EDGE('',*,*,#4668,.T.);
#5776=ORIENTED_EDGE('',*,*,#4624,.F.);
#5777=ORIENTED_EDGE('',*,*,#4670,.F.);
#5778=ORIENTED_EDGE('',*,*,#4671,.T.);
#5779=ORIENTED_EDGE('',*,*,#4670,.T.);
#5780=ORIENTED_EDGE('',*,*,#4623,.F.);
#5781=ORIENTED_EDGE('',*,*,#4672,.F.);
#5782=ORIENTED_EDGE('',*,*,#4673,.T.);
#5783=ORIENTED_EDGE('',*,*,#4672,.T.);
#5784=ORIENTED_EDGE('',*,*,#4622,.F.);
#5785=ORIENTED_EDGE('',*,*,#4667,.F.);
#5786=ORIENTED_EDGE('',*,*,#4673,.F.);
#5787=ORIENTED_EDGE('',*,*,#4666,.F.);
#5788=ORIENTED_EDGE('',*,*,#4669,.F.);
#5789=ORIENTED_EDGE('',*,*,#4671,.F.);
#5790=ORIENTED_EDGE('',*,*,#4660,.T.);
#5791=ORIENTED_EDGE('',*,*,#4665,.T.);
#5792=ORIENTED_EDGE('',*,*,#4663,.T.);
#5793=ORIENTED_EDGE('',*,*,#4664,.T.);
#5794=ORIENTED_EDGE('',*,*,#4652,.T.);
#5795=ORIENTED_EDGE('',*,*,#4657,.T.);
#5796=ORIENTED_EDGE('',*,*,#4655,.T.);
#5797=ORIENTED_EDGE('',*,*,#4656,.T.);
#5798=ORIENTED_EDGE('',*,*,#4644,.T.);
#5799=ORIENTED_EDGE('',*,*,#4649,.T.);
#5800=ORIENTED_EDGE('',*,*,#4647,.T.);
#5801=ORIENTED_EDGE('',*,*,#4648,.T.);
#5802=ORIENTED_EDGE('',*,*,#4617,.T.);
#5803=ORIENTED_EDGE('',*,*,#4641,.T.);
#5804=ORIENTED_EDGE('',*,*,#4621,.T.);
#5805=ORIENTED_EDGE('',*,*,#4640,.T.);
#5806=ORIENTED_EDGE('',*,*,#4611,.T.);
#5807=ORIENTED_EDGE('',*,*,#4608,.T.);
#5808=ORIENTED_EDGE('',*,*,#4605,.T.);
#5809=ORIENTED_EDGE('',*,*,#4602,.T.);
#5810=ORIENTED_EDGE('',*,*,#4674,.F.);
#5811=ORIENTED_EDGE('',*,*,#4675,.T.);
#5812=ORIENTED_EDGE('',*,*,#4676,.F.);
#5813=ORIENTED_EDGE('',*,*,#4675,.F.);
#5814=ORIENTED_EDGE('',*,*,#4677,.F.);
#5815=ORIENTED_EDGE('',*,*,#4678,.T.);
#5816=ORIENTED_EDGE('',*,*,#4679,.F.);
#5817=ORIENTED_EDGE('',*,*,#4678,.F.);
#5818=ORIENTED_EDGE('',*,*,#4680,.F.);
#5819=ORIENTED_EDGE('',*,*,#4681,.T.);
#5820=ORIENTED_EDGE('',*,*,#4682,.F.);
#5821=ORIENTED_EDGE('',*,*,#4681,.F.);
#5822=ORIENTED_EDGE('',*,*,#4683,.F.);
#5823=ORIENTED_EDGE('',*,*,#4684,.T.);
#5824=ORIENTED_EDGE('',*,*,#4685,.F.);
#5825=ORIENTED_EDGE('',*,*,#4684,.F.);
#5826=ORIENTED_EDGE('',*,*,#4686,.F.);
#5827=ORIENTED_EDGE('',*,*,#4687,.T.);
#5828=ORIENTED_EDGE('',*,*,#4688,.F.);
#5829=ORIENTED_EDGE('',*,*,#4687,.F.);
#5830=ORIENTED_EDGE('',*,*,#4689,.F.);
#5831=ORIENTED_EDGE('',*,*,#4690,.T.);
#5832=ORIENTED_EDGE('',*,*,#4691,.F.);
#5833=ORIENTED_EDGE('',*,*,#4690,.F.);
#5834=ORIENTED_EDGE('',*,*,#4692,.F.);
#5835=ORIENTED_EDGE('',*,*,#4693,.T.);
#5836=ORIENTED_EDGE('',*,*,#4694,.F.);
#5837=ORIENTED_EDGE('',*,*,#4693,.F.);
#5838=ORIENTED_EDGE('',*,*,#4695,.F.);
#5839=ORIENTED_EDGE('',*,*,#4696,.F.);
#5840=ORIENTED_EDGE('',*,*,#4697,.T.);
#5841=ORIENTED_EDGE('',*,*,#4698,.F.);
#5842=ORIENTED_EDGE('',*,*,#4694,.T.);
#5843=ORIENTED_EDGE('',*,*,#4699,.F.);
#5844=ORIENTED_EDGE('',*,*,#4700,.F.);
#5845=ORIENTED_EDGE('',*,*,#4701,.F.);
#5846=ORIENTED_EDGE('',*,*,#4702,.F.);
#5847=ORIENTED_EDGE('',*,*,#4691,.T.);
#5848=ORIENTED_EDGE('',*,*,#4703,.F.);
#5849=ORIENTED_EDGE('',*,*,#4701,.T.);
#5850=ORIENTED_EDGE('',*,*,#4704,.F.);
#5851=ORIENTED_EDGE('',*,*,#4705,.F.);
#5852=ORIENTED_EDGE('',*,*,#4706,.F.);
#5853=ORIENTED_EDGE('',*,*,#4707,.T.);
#5854=ORIENTED_EDGE('',*,*,#4708,.F.);
#5855=ORIENTED_EDGE('',*,*,#4697,.F.);
#5856=ORIENTED_EDGE('',*,*,#4709,.T.);
#5857=ORIENTED_EDGE('',*,*,#4710,.F.);
#5858=ORIENTED_EDGE('',*,*,#4711,.F.);
#5859=ORIENTED_EDGE('',*,*,#4702,.T.);
#5860=ORIENTED_EDGE('',*,*,#4703,.T.);
#5861=ORIENTED_EDGE('',*,*,#4712,.T.);
#5862=ORIENTED_EDGE('',*,*,#4706,.T.);
#5863=ORIENTED_EDGE('',*,*,#4696,.T.);
#5864=ORIENTED_EDGE('',*,*,#4686,.T.);
#5865=ORIENTED_EDGE('',*,*,#4683,.T.);
#5866=ORIENTED_EDGE('',*,*,#4680,.T.);
#5867=ORIENTED_EDGE('',*,*,#4677,.T.);
#5868=ORIENTED_EDGE('',*,*,#4674,.T.);
#5869=ORIENTED_EDGE('',*,*,#4695,.T.);
#5870=ORIENTED_EDGE('',*,*,#4713,.T.);
#5871=ORIENTED_EDGE('',*,*,#4714,.F.);
#5872=ORIENTED_EDGE('',*,*,#4709,.F.);
#5873=ORIENTED_EDGE('',*,*,#4715,.T.);
#5874=ORIENTED_EDGE('',*,*,#4716,.F.);
#5875=ORIENTED_EDGE('',*,*,#4713,.F.);
#5876=ORIENTED_EDGE('',*,*,#4698,.T.);
#5877=ORIENTED_EDGE('',*,*,#4708,.T.);
#5878=ORIENTED_EDGE('',*,*,#4717,.T.);
#5879=ORIENTED_EDGE('',*,*,#4704,.T.);
#5880=ORIENTED_EDGE('',*,*,#4700,.T.);
#5881=ORIENTED_EDGE('',*,*,#4688,.T.);
#5882=ORIENTED_EDGE('',*,*,#4685,.T.);
#5883=ORIENTED_EDGE('',*,*,#4682,.T.);
#5884=ORIENTED_EDGE('',*,*,#4679,.T.);
#5885=ORIENTED_EDGE('',*,*,#4676,.T.);
#5886=ORIENTED_EDGE('',*,*,#4699,.T.);
#5887=ORIENTED_EDGE('',*,*,#4711,.T.);
#5888=ORIENTED_EDGE('',*,*,#4718,.F.);
#5889=ORIENTED_EDGE('',*,*,#4715,.F.);
#5890=ORIENTED_EDGE('',*,*,#4718,.T.);
#5891=ORIENTED_EDGE('',*,*,#4710,.T.);
#5892=ORIENTED_EDGE('',*,*,#4714,.T.);
#5893=ORIENTED_EDGE('',*,*,#4716,.T.);
#5894=ORIENTED_EDGE('',*,*,#4717,.F.);
#5895=ORIENTED_EDGE('',*,*,#4707,.F.);
#5896=ORIENTED_EDGE('',*,*,#4712,.F.);
#5897=ORIENTED_EDGE('',*,*,#4705,.T.);
#5898=ORIENTED_EDGE('',*,*,#4689,.T.);
#5899=ORIENTED_EDGE('',*,*,#4692,.T.);
#5900=ORIENTED_EDGE('',*,*,#4719,.F.);
#5901=ORIENTED_EDGE('',*,*,#4720,.T.);
#5902=ORIENTED_EDGE('',*,*,#4721,.F.);
#5903=ORIENTED_EDGE('',*,*,#4720,.F.);
#5904=ORIENTED_EDGE('',*,*,#4722,.F.);
#5905=ORIENTED_EDGE('',*,*,#4723,.T.);
#5906=ORIENTED_EDGE('',*,*,#4724,.F.);
#5907=ORIENTED_EDGE('',*,*,#4723,.F.);
#5908=ORIENTED_EDGE('',*,*,#4725,.F.);
#5909=ORIENTED_EDGE('',*,*,#4726,.T.);
#5910=ORIENTED_EDGE('',*,*,#4727,.F.);
#5911=ORIENTED_EDGE('',*,*,#4726,.F.);
#5912=ORIENTED_EDGE('',*,*,#4728,.F.);
#5913=ORIENTED_EDGE('',*,*,#4729,.T.);
#5914=ORIENTED_EDGE('',*,*,#4730,.F.);
#5915=ORIENTED_EDGE('',*,*,#4729,.F.);
#5916=ORIENTED_EDGE('',*,*,#4731,.F.);
#5917=ORIENTED_EDGE('',*,*,#4732,.T.);
#5918=ORIENTED_EDGE('',*,*,#4733,.F.);
#5919=ORIENTED_EDGE('',*,*,#4732,.F.);
#5920=ORIENTED_EDGE('',*,*,#4731,.T.);
#5921=ORIENTED_EDGE('',*,*,#4734,.T.);
#5922=ORIENTED_EDGE('',*,*,#4734,.F.);
#5923=ORIENTED_EDGE('',*,*,#4735,.T.);
#5924=ORIENTED_EDGE('',*,*,#4736,.T.);
#5925=ORIENTED_EDGE('',*,*,#4735,.F.);
#5926=ORIENTED_EDGE('',*,*,#4737,.F.);
#5927=ORIENTED_EDGE('',*,*,#4738,.T.);
#5928=ORIENTED_EDGE('',*,*,#4739,.T.);
#5929=ORIENTED_EDGE('',*,*,#4738,.F.);
#5930=ORIENTED_EDGE('',*,*,#4737,.T.);
#5931=ORIENTED_EDGE('',*,*,#4733,.T.);
#5932=ORIENTED_EDGE('',*,*,#4730,.T.);
#5933=ORIENTED_EDGE('',*,*,#4727,.T.);
#5934=ORIENTED_EDGE('',*,*,#4724,.T.);
#5935=ORIENTED_EDGE('',*,*,#4721,.T.);
#5936=ORIENTED_EDGE('',*,*,#4739,.F.);
#5937=ORIENTED_EDGE('',*,*,#4736,.F.);
#5938=ORIENTED_EDGE('',*,*,#4728,.T.);
#5939=ORIENTED_EDGE('',*,*,#4725,.T.);
#5940=ORIENTED_EDGE('',*,*,#4722,.T.);
#5941=ORIENTED_EDGE('',*,*,#4719,.T.);
#5942=ORIENTED_EDGE('',*,*,#4740,.F.);
#5943=ORIENTED_EDGE('',*,*,#4741,.T.);
#5944=ORIENTED_EDGE('',*,*,#4742,.F.);
#5945=ORIENTED_EDGE('',*,*,#4741,.F.);
#5946=ORIENTED_EDGE('',*,*,#4743,.F.);
#5947=ORIENTED_EDGE('',*,*,#4744,.T.);
#5948=ORIENTED_EDGE('',*,*,#4745,.F.);
#5949=ORIENTED_EDGE('',*,*,#4744,.F.);
#5950=ORIENTED_EDGE('',*,*,#4746,.F.);
#5951=ORIENTED_EDGE('',*,*,#4747,.T.);
#5952=ORIENTED_EDGE('',*,*,#4748,.F.);
#5953=ORIENTED_EDGE('',*,*,#4747,.F.);
#5954=ORIENTED_EDGE('',*,*,#4749,.F.);
#5955=ORIENTED_EDGE('',*,*,#4750,.T.);
#5956=ORIENTED_EDGE('',*,*,#4751,.F.);
#5957=ORIENTED_EDGE('',*,*,#4750,.F.);
#5958=ORIENTED_EDGE('',*,*,#4752,.F.);
#5959=ORIENTED_EDGE('',*,*,#4753,.T.);
#5960=ORIENTED_EDGE('',*,*,#4754,.T.);
#5961=ORIENTED_EDGE('',*,*,#4753,.F.);
#5962=ORIENTED_EDGE('',*,*,#4754,.F.);
#5963=ORIENTED_EDGE('',*,*,#4755,.F.);
#5964=ORIENTED_EDGE('',*,*,#4756,.F.);
#5965=ORIENTED_EDGE('',*,*,#4757,.T.);
#5966=ORIENTED_EDGE('',*,*,#4755,.T.);
#5967=ORIENTED_EDGE('',*,*,#4757,.F.);
#5968=ORIENTED_EDGE('',*,*,#4758,.F.);
#5969=ORIENTED_EDGE('',*,*,#4759,.T.);
#5970=ORIENTED_EDGE('',*,*,#4760,.T.);
#5971=ORIENTED_EDGE('',*,*,#4759,.F.);
#5972=ORIENTED_EDGE('',*,*,#4758,.T.);
#5973=ORIENTED_EDGE('',*,*,#4756,.T.);
#5974=ORIENTED_EDGE('',*,*,#4751,.T.);
#5975=ORIENTED_EDGE('',*,*,#4748,.T.);
#5976=ORIENTED_EDGE('',*,*,#4745,.T.);
#5977=ORIENTED_EDGE('',*,*,#4742,.T.);
#5978=ORIENTED_EDGE('',*,*,#4760,.F.);
#5979=ORIENTED_EDGE('',*,*,#4752,.T.);
#5980=ORIENTED_EDGE('',*,*,#4749,.T.);
#5981=ORIENTED_EDGE('',*,*,#4746,.T.);
#5982=ORIENTED_EDGE('',*,*,#4743,.T.);
#5983=ORIENTED_EDGE('',*,*,#4740,.T.);
#5984=ORIENTED_EDGE('',*,*,#4761,.F.);
#5985=ORIENTED_EDGE('',*,*,#4762,.T.);
#5986=ORIENTED_EDGE('',*,*,#4763,.F.);
#5987=ORIENTED_EDGE('',*,*,#4762,.F.);
#5988=ORIENTED_EDGE('',*,*,#4764,.F.);
#5989=ORIENTED_EDGE('',*,*,#4765,.T.);
#5990=ORIENTED_EDGE('',*,*,#4766,.F.);
#5991=ORIENTED_EDGE('',*,*,#4765,.F.);
#5992=ORIENTED_EDGE('',*,*,#4767,.F.);
#5993=ORIENTED_EDGE('',*,*,#4768,.T.);
#5994=ORIENTED_EDGE('',*,*,#4769,.F.);
#5995=ORIENTED_EDGE('',*,*,#4768,.F.);
#5996=ORIENTED_EDGE('',*,*,#4770,.F.);
#5997=ORIENTED_EDGE('',*,*,#4771,.T.);
#5998=ORIENTED_EDGE('',*,*,#4772,.F.);
#5999=ORIENTED_EDGE('',*,*,#4771,.F.);
#6000=ORIENTED_EDGE('',*,*,#4773,.F.);
#6001=ORIENTED_EDGE('',*,*,#4774,.T.);
#6002=ORIENTED_EDGE('',*,*,#4775,.F.);
#6003=ORIENTED_EDGE('',*,*,#4774,.F.);
#6004=ORIENTED_EDGE('',*,*,#4776,.F.);
#6005=ORIENTED_EDGE('',*,*,#4777,.T.);
#6006=ORIENTED_EDGE('',*,*,#4778,.F.);
#6007=ORIENTED_EDGE('',*,*,#4777,.F.);
#6008=ORIENTED_EDGE('',*,*,#4779,.F.);
#6009=ORIENTED_EDGE('',*,*,#4780,.T.);
#6010=ORIENTED_EDGE('',*,*,#4781,.F.);
#6011=ORIENTED_EDGE('',*,*,#4780,.F.);
#6012=ORIENTED_EDGE('',*,*,#4782,.F.);
#6013=ORIENTED_EDGE('',*,*,#4783,.F.);
#6014=ORIENTED_EDGE('',*,*,#4784,.T.);
#6015=ORIENTED_EDGE('',*,*,#4785,.F.);
#6016=ORIENTED_EDGE('',*,*,#4781,.T.);
#6017=ORIENTED_EDGE('',*,*,#4786,.F.);
#6018=ORIENTED_EDGE('',*,*,#4787,.F.);
#6019=ORIENTED_EDGE('',*,*,#4788,.F.);
#6020=ORIENTED_EDGE('',*,*,#4789,.F.);
#6021=ORIENTED_EDGE('',*,*,#4778,.T.);
#6022=ORIENTED_EDGE('',*,*,#4790,.F.);
#6023=ORIENTED_EDGE('',*,*,#4788,.T.);
#6024=ORIENTED_EDGE('',*,*,#4791,.F.);
#6025=ORIENTED_EDGE('',*,*,#4792,.F.);
#6026=ORIENTED_EDGE('',*,*,#4793,.F.);
#6027=ORIENTED_EDGE('',*,*,#4794,.T.);
#6028=ORIENTED_EDGE('',*,*,#4795,.F.);
#6029=ORIENTED_EDGE('',*,*,#4784,.F.);
#6030=ORIENTED_EDGE('',*,*,#4796,.T.);
#6031=ORIENTED_EDGE('',*,*,#4797,.F.);
#6032=ORIENTED_EDGE('',*,*,#4798,.F.);
#6033=ORIENTED_EDGE('',*,*,#4789,.T.);
#6034=ORIENTED_EDGE('',*,*,#4790,.T.);
#6035=ORIENTED_EDGE('',*,*,#4799,.T.);
#6036=ORIENTED_EDGE('',*,*,#4793,.T.);
#6037=ORIENTED_EDGE('',*,*,#4783,.T.);
#6038=ORIENTED_EDGE('',*,*,#4773,.T.);
#6039=ORIENTED_EDGE('',*,*,#4770,.T.);
#6040=ORIENTED_EDGE('',*,*,#4767,.T.);
#6041=ORIENTED_EDGE('',*,*,#4764,.T.);
#6042=ORIENTED_EDGE('',*,*,#4761,.T.);
#6043=ORIENTED_EDGE('',*,*,#4782,.T.);
#6044=ORIENTED_EDGE('',*,*,#4800,.T.);
#6045=ORIENTED_EDGE('',*,*,#4801,.F.);
#6046=ORIENTED_EDGE('',*,*,#4796,.F.);
#6047=ORIENTED_EDGE('',*,*,#4802,.T.);
#6048=ORIENTED_EDGE('',*,*,#4803,.F.);
#6049=ORIENTED_EDGE('',*,*,#4800,.F.);
#6050=ORIENTED_EDGE('',*,*,#4785,.T.);
#6051=ORIENTED_EDGE('',*,*,#4795,.T.);
#6052=ORIENTED_EDGE('',*,*,#4804,.T.);
#6053=ORIENTED_EDGE('',*,*,#4791,.T.);
#6054=ORIENTED_EDGE('',*,*,#4787,.T.);
#6055=ORIENTED_EDGE('',*,*,#4775,.T.);
#6056=ORIENTED_EDGE('',*,*,#4772,.T.);
#6057=ORIENTED_EDGE('',*,*,#4769,.T.);
#6058=ORIENTED_EDGE('',*,*,#4766,.T.);
#6059=ORIENTED_EDGE('',*,*,#4763,.T.);
#6060=ORIENTED_EDGE('',*,*,#4786,.T.);
#6061=ORIENTED_EDGE('',*,*,#4798,.T.);
#6062=ORIENTED_EDGE('',*,*,#4805,.F.);
#6063=ORIENTED_EDGE('',*,*,#4802,.F.);
#6064=ORIENTED_EDGE('',*,*,#4805,.T.);
#6065=ORIENTED_EDGE('',*,*,#4797,.T.);
#6066=ORIENTED_EDGE('',*,*,#4801,.T.);
#6067=ORIENTED_EDGE('',*,*,#4803,.T.);
#6068=ORIENTED_EDGE('',*,*,#4804,.F.);
#6069=ORIENTED_EDGE('',*,*,#4794,.F.);
#6070=ORIENTED_EDGE('',*,*,#4799,.F.);
#6071=ORIENTED_EDGE('',*,*,#4792,.T.);
#6072=ORIENTED_EDGE('',*,*,#4776,.T.);
#6073=ORIENTED_EDGE('',*,*,#4779,.T.);
#6074=ORIENTED_EDGE('',*,*,#4806,.F.);
#6075=ORIENTED_EDGE('',*,*,#4807,.T.);
#6076=ORIENTED_EDGE('',*,*,#4808,.F.);
#6077=ORIENTED_EDGE('',*,*,#4807,.F.);
#6078=ORIENTED_EDGE('',*,*,#4809,.F.);
#6079=ORIENTED_EDGE('',*,*,#4810,.T.);
#6080=ORIENTED_EDGE('',*,*,#4811,.F.);
#6081=ORIENTED_EDGE('',*,*,#4810,.F.);
#6082=ORIENTED_EDGE('',*,*,#4812,.F.);
#6083=ORIENTED_EDGE('',*,*,#4813,.T.);
#6084=ORIENTED_EDGE('',*,*,#4814,.F.);
#6085=ORIENTED_EDGE('',*,*,#4813,.F.);
#6086=ORIENTED_EDGE('',*,*,#4815,.F.);
#6087=ORIENTED_EDGE('',*,*,#4816,.T.);
#6088=ORIENTED_EDGE('',*,*,#4817,.F.);
#6089=ORIENTED_EDGE('',*,*,#4816,.F.);
#6090=ORIENTED_EDGE('',*,*,#4818,.F.);
#6091=ORIENTED_EDGE('',*,*,#4819,.T.);
#6092=ORIENTED_EDGE('',*,*,#4820,.F.);
#6093=ORIENTED_EDGE('',*,*,#4819,.F.);
#6094=ORIENTED_EDGE('',*,*,#4818,.T.);
#6095=ORIENTED_EDGE('',*,*,#4821,.T.);
#6096=ORIENTED_EDGE('',*,*,#4821,.F.);
#6097=ORIENTED_EDGE('',*,*,#4822,.T.);
#6098=ORIENTED_EDGE('',*,*,#4823,.T.);
#6099=ORIENTED_EDGE('',*,*,#4822,.F.);
#6100=ORIENTED_EDGE('',*,*,#4824,.F.);
#6101=ORIENTED_EDGE('',*,*,#4825,.T.);
#6102=ORIENTED_EDGE('',*,*,#4826,.T.);
#6103=ORIENTED_EDGE('',*,*,#4825,.F.);
#6104=ORIENTED_EDGE('',*,*,#4824,.T.);
#6105=ORIENTED_EDGE('',*,*,#4820,.T.);
#6106=ORIENTED_EDGE('',*,*,#4817,.T.);
#6107=ORIENTED_EDGE('',*,*,#4814,.T.);
#6108=ORIENTED_EDGE('',*,*,#4811,.T.);
#6109=ORIENTED_EDGE('',*,*,#4808,.T.);
#6110=ORIENTED_EDGE('',*,*,#4826,.F.);
#6111=ORIENTED_EDGE('',*,*,#4823,.F.);
#6112=ORIENTED_EDGE('',*,*,#4815,.T.);
#6113=ORIENTED_EDGE('',*,*,#4812,.T.);
#6114=ORIENTED_EDGE('',*,*,#4809,.T.);
#6115=ORIENTED_EDGE('',*,*,#4806,.T.);
#6116=ORIENTED_EDGE('',*,*,#4827,.F.);
#6117=ORIENTED_EDGE('',*,*,#4828,.T.);
#6118=ORIENTED_EDGE('',*,*,#4829,.F.);
#6119=ORIENTED_EDGE('',*,*,#4828,.F.);
#6120=ORIENTED_EDGE('',*,*,#4830,.F.);
#6121=ORIENTED_EDGE('',*,*,#4831,.T.);
#6122=ORIENTED_EDGE('',*,*,#4832,.F.);
#6123=ORIENTED_EDGE('',*,*,#4831,.F.);
#6124=ORIENTED_EDGE('',*,*,#4833,.F.);
#6125=ORIENTED_EDGE('',*,*,#4834,.T.);
#6126=ORIENTED_EDGE('',*,*,#4835,.F.);
#6127=ORIENTED_EDGE('',*,*,#4834,.F.);
#6128=ORIENTED_EDGE('',*,*,#4836,.F.);
#6129=ORIENTED_EDGE('',*,*,#4837,.T.);
#6130=ORIENTED_EDGE('',*,*,#4838,.F.);
#6131=ORIENTED_EDGE('',*,*,#4837,.F.);
#6132=ORIENTED_EDGE('',*,*,#4839,.F.);
#6133=ORIENTED_EDGE('',*,*,#4840,.T.);
#6134=ORIENTED_EDGE('',*,*,#4841,.T.);
#6135=ORIENTED_EDGE('',*,*,#4840,.F.);
#6136=ORIENTED_EDGE('',*,*,#4841,.F.);
#6137=ORIENTED_EDGE('',*,*,#4842,.F.);
#6138=ORIENTED_EDGE('',*,*,#4843,.F.);
#6139=ORIENTED_EDGE('',*,*,#4844,.T.);
#6140=ORIENTED_EDGE('',*,*,#4842,.T.);
#6141=ORIENTED_EDGE('',*,*,#4844,.F.);
#6142=ORIENTED_EDGE('',*,*,#4845,.F.);
#6143=ORIENTED_EDGE('',*,*,#4846,.T.);
#6144=ORIENTED_EDGE('',*,*,#4847,.T.);
#6145=ORIENTED_EDGE('',*,*,#4846,.F.);
#6146=ORIENTED_EDGE('',*,*,#4845,.T.);
#6147=ORIENTED_EDGE('',*,*,#4843,.T.);
#6148=ORIENTED_EDGE('',*,*,#4838,.T.);
#6149=ORIENTED_EDGE('',*,*,#4835,.T.);
#6150=ORIENTED_EDGE('',*,*,#4832,.T.);
#6151=ORIENTED_EDGE('',*,*,#4829,.T.);
#6152=ORIENTED_EDGE('',*,*,#4847,.F.);
#6153=ORIENTED_EDGE('',*,*,#4839,.T.);
#6154=ORIENTED_EDGE('',*,*,#4836,.T.);
#6155=ORIENTED_EDGE('',*,*,#4833,.T.);
#6156=ORIENTED_EDGE('',*,*,#4830,.T.);
#6157=ORIENTED_EDGE('',*,*,#4827,.T.);
#6158=ORIENTED_EDGE('',*,*,#4848,.F.);
#6159=ORIENTED_EDGE('',*,*,#4849,.T.);
#6160=ORIENTED_EDGE('',*,*,#4850,.F.);
#6161=ORIENTED_EDGE('',*,*,#4849,.F.);
#6162=ORIENTED_EDGE('',*,*,#4851,.F.);
#6163=ORIENTED_EDGE('',*,*,#4852,.T.);
#6164=ORIENTED_EDGE('',*,*,#4853,.F.);
#6165=ORIENTED_EDGE('',*,*,#4852,.F.);
#6166=ORIENTED_EDGE('',*,*,#4854,.F.);
#6167=ORIENTED_EDGE('',*,*,#4855,.T.);
#6168=ORIENTED_EDGE('',*,*,#4856,.F.);
#6169=ORIENTED_EDGE('',*,*,#4855,.F.);
#6170=ORIENTED_EDGE('',*,*,#4857,.F.);
#6171=ORIENTED_EDGE('',*,*,#4858,.T.);
#6172=ORIENTED_EDGE('',*,*,#4859,.F.);
#6173=ORIENTED_EDGE('',*,*,#4858,.F.);
#6174=ORIENTED_EDGE('',*,*,#4860,.F.);
#6175=ORIENTED_EDGE('',*,*,#4861,.T.);
#6176=ORIENTED_EDGE('',*,*,#4862,.F.);
#6177=ORIENTED_EDGE('',*,*,#4861,.F.);
#6178=ORIENTED_EDGE('',*,*,#4863,.F.);
#6179=ORIENTED_EDGE('',*,*,#4864,.T.);
#6180=ORIENTED_EDGE('',*,*,#4865,.F.);
#6181=ORIENTED_EDGE('',*,*,#4864,.F.);
#6182=ORIENTED_EDGE('',*,*,#4866,.F.);
#6183=ORIENTED_EDGE('',*,*,#4867,.T.);
#6184=ORIENTED_EDGE('',*,*,#4868,.F.);
#6185=ORIENTED_EDGE('',*,*,#4867,.F.);
#6186=ORIENTED_EDGE('',*,*,#4869,.F.);
#6187=ORIENTED_EDGE('',*,*,#4870,.F.);
#6188=ORIENTED_EDGE('',*,*,#4871,.T.);
#6189=ORIENTED_EDGE('',*,*,#4872,.F.);
#6190=ORIENTED_EDGE('',*,*,#4868,.T.);
#6191=ORIENTED_EDGE('',*,*,#4873,.F.);
#6192=ORIENTED_EDGE('',*,*,#4874,.F.);
#6193=ORIENTED_EDGE('',*,*,#4875,.F.);
#6194=ORIENTED_EDGE('',*,*,#4876,.F.);
#6195=ORIENTED_EDGE('',*,*,#4865,.T.);
#6196=ORIENTED_EDGE('',*,*,#4877,.F.);
#6197=ORIENTED_EDGE('',*,*,#4875,.T.);
#6198=ORIENTED_EDGE('',*,*,#4878,.F.);
#6199=ORIENTED_EDGE('',*,*,#4879,.F.);
#6200=ORIENTED_EDGE('',*,*,#4880,.F.);
#6201=ORIENTED_EDGE('',*,*,#4881,.T.);
#6202=ORIENTED_EDGE('',*,*,#4882,.F.);
#6203=ORIENTED_EDGE('',*,*,#4871,.F.);
#6204=ORIENTED_EDGE('',*,*,#4883,.T.);
#6205=ORIENTED_EDGE('',*,*,#4884,.F.);
#6206=ORIENTED_EDGE('',*,*,#4885,.F.);
#6207=ORIENTED_EDGE('',*,*,#4876,.T.);
#6208=ORIENTED_EDGE('',*,*,#4877,.T.);
#6209=ORIENTED_EDGE('',*,*,#4886,.T.);
#6210=ORIENTED_EDGE('',*,*,#4880,.T.);
#6211=ORIENTED_EDGE('',*,*,#4870,.T.);
#6212=ORIENTED_EDGE('',*,*,#4869,.T.);
#6213=ORIENTED_EDGE('',*,*,#4887,.T.);
#6214=ORIENTED_EDGE('',*,*,#4888,.F.);
#6215=ORIENTED_EDGE('',*,*,#4883,.F.);
#6216=ORIENTED_EDGE('',*,*,#4862,.T.);
#6217=ORIENTED_EDGE('',*,*,#4859,.T.);
#6218=ORIENTED_EDGE('',*,*,#4856,.T.);
#6219=ORIENTED_EDGE('',*,*,#4853,.T.);
#6220=ORIENTED_EDGE('',*,*,#4850,.T.);
#6221=ORIENTED_EDGE('',*,*,#4889,.T.);
#6222=ORIENTED_EDGE('',*,*,#4890,.F.);
#6223=ORIENTED_EDGE('',*,*,#4887,.F.);
#6224=ORIENTED_EDGE('',*,*,#4872,.T.);
#6225=ORIENTED_EDGE('',*,*,#4882,.T.);
#6226=ORIENTED_EDGE('',*,*,#4891,.T.);
#6227=ORIENTED_EDGE('',*,*,#4878,.T.);
#6228=ORIENTED_EDGE('',*,*,#4874,.T.);
#6229=ORIENTED_EDGE('',*,*,#4873,.T.);
#6230=ORIENTED_EDGE('',*,*,#4885,.T.);
#6231=ORIENTED_EDGE('',*,*,#4892,.F.);
#6232=ORIENTED_EDGE('',*,*,#4889,.F.);
#6233=ORIENTED_EDGE('',*,*,#4860,.T.);
#6234=ORIENTED_EDGE('',*,*,#4857,.T.);
#6235=ORIENTED_EDGE('',*,*,#4854,.T.);
#6236=ORIENTED_EDGE('',*,*,#4851,.T.);
#6237=ORIENTED_EDGE('',*,*,#4848,.T.);
#6238=ORIENTED_EDGE('',*,*,#4892,.T.);
#6239=ORIENTED_EDGE('',*,*,#4884,.T.);
#6240=ORIENTED_EDGE('',*,*,#4888,.T.);
#6241=ORIENTED_EDGE('',*,*,#4890,.T.);
#6242=ORIENTED_EDGE('',*,*,#4891,.F.);
#6243=ORIENTED_EDGE('',*,*,#4881,.F.);
#6244=ORIENTED_EDGE('',*,*,#4886,.F.);
#6245=ORIENTED_EDGE('',*,*,#4879,.T.);
#6246=ORIENTED_EDGE('',*,*,#4863,.T.);
#6247=ORIENTED_EDGE('',*,*,#4866,.T.);
#6248=ORIENTED_EDGE('',*,*,#4893,.F.);
#6249=ORIENTED_EDGE('',*,*,#4894,.T.);
#6250=ORIENTED_EDGE('',*,*,#4895,.F.);
#6251=ORIENTED_EDGE('',*,*,#4894,.F.);
#6252=ORIENTED_EDGE('',*,*,#4896,.F.);
#6253=ORIENTED_EDGE('',*,*,#4897,.T.);
#6254=ORIENTED_EDGE('',*,*,#4898,.F.);
#6255=ORIENTED_EDGE('',*,*,#4897,.F.);
#6256=ORIENTED_EDGE('',*,*,#4899,.F.);
#6257=ORIENTED_EDGE('',*,*,#4900,.T.);
#6258=ORIENTED_EDGE('',*,*,#4901,.F.);
#6259=ORIENTED_EDGE('',*,*,#4900,.F.);
#6260=ORIENTED_EDGE('',*,*,#4902,.F.);
#6261=ORIENTED_EDGE('',*,*,#4903,.T.);
#6262=ORIENTED_EDGE('',*,*,#4904,.F.);
#6263=ORIENTED_EDGE('',*,*,#4903,.F.);
#6264=ORIENTED_EDGE('',*,*,#4905,.F.);
#6265=ORIENTED_EDGE('',*,*,#4906,.T.);
#6266=ORIENTED_EDGE('',*,*,#4907,.F.);
#6267=ORIENTED_EDGE('',*,*,#4906,.F.);
#6268=ORIENTED_EDGE('',*,*,#4905,.T.);
#6269=ORIENTED_EDGE('',*,*,#4908,.T.);
#6270=ORIENTED_EDGE('',*,*,#4908,.F.);
#6271=ORIENTED_EDGE('',*,*,#4909,.T.);
#6272=ORIENTED_EDGE('',*,*,#4910,.T.);
#6273=ORIENTED_EDGE('',*,*,#4909,.F.);
#6274=ORIENTED_EDGE('',*,*,#4911,.F.);
#6275=ORIENTED_EDGE('',*,*,#4912,.T.);
#6276=ORIENTED_EDGE('',*,*,#4913,.T.);
#6277=ORIENTED_EDGE('',*,*,#4912,.F.);
#6278=ORIENTED_EDGE('',*,*,#4911,.T.);
#6279=ORIENTED_EDGE('',*,*,#4907,.T.);
#6280=ORIENTED_EDGE('',*,*,#4904,.T.);
#6281=ORIENTED_EDGE('',*,*,#4901,.T.);
#6282=ORIENTED_EDGE('',*,*,#4898,.T.);
#6283=ORIENTED_EDGE('',*,*,#4895,.T.);
#6284=ORIENTED_EDGE('',*,*,#4913,.F.);
#6285=ORIENTED_EDGE('',*,*,#4910,.F.);
#6286=ORIENTED_EDGE('',*,*,#4902,.T.);
#6287=ORIENTED_EDGE('',*,*,#4899,.T.);
#6288=ORIENTED_EDGE('',*,*,#4896,.T.);
#6289=ORIENTED_EDGE('',*,*,#4893,.T.);
#6290=ORIENTED_EDGE('',*,*,#4914,.F.);
#6291=ORIENTED_EDGE('',*,*,#4915,.T.);
#6292=ORIENTED_EDGE('',*,*,#4916,.F.);
#6293=ORIENTED_EDGE('',*,*,#4915,.F.);
#6294=ORIENTED_EDGE('',*,*,#4917,.F.);
#6295=ORIENTED_EDGE('',*,*,#4918,.T.);
#6296=ORIENTED_EDGE('',*,*,#4919,.F.);
#6297=ORIENTED_EDGE('',*,*,#4918,.F.);
#6298=ORIENTED_EDGE('',*,*,#4920,.F.);
#6299=ORIENTED_EDGE('',*,*,#4921,.T.);
#6300=ORIENTED_EDGE('',*,*,#4922,.F.);
#6301=ORIENTED_EDGE('',*,*,#4921,.F.);
#6302=ORIENTED_EDGE('',*,*,#4923,.F.);
#6303=ORIENTED_EDGE('',*,*,#4924,.T.);
#6304=ORIENTED_EDGE('',*,*,#4925,.F.);
#6305=ORIENTED_EDGE('',*,*,#4924,.F.);
#6306=ORIENTED_EDGE('',*,*,#4926,.F.);
#6307=ORIENTED_EDGE('',*,*,#4927,.T.);
#6308=ORIENTED_EDGE('',*,*,#4928,.T.);
#6309=ORIENTED_EDGE('',*,*,#4927,.F.);
#6310=ORIENTED_EDGE('',*,*,#4928,.F.);
#6311=ORIENTED_EDGE('',*,*,#4929,.F.);
#6312=ORIENTED_EDGE('',*,*,#4930,.F.);
#6313=ORIENTED_EDGE('',*,*,#4931,.T.);
#6314=ORIENTED_EDGE('',*,*,#4929,.T.);
#6315=ORIENTED_EDGE('',*,*,#4931,.F.);
#6316=ORIENTED_EDGE('',*,*,#4932,.F.);
#6317=ORIENTED_EDGE('',*,*,#4933,.T.);
#6318=ORIENTED_EDGE('',*,*,#4934,.T.);
#6319=ORIENTED_EDGE('',*,*,#4933,.F.);
#6320=ORIENTED_EDGE('',*,*,#4932,.T.);
#6321=ORIENTED_EDGE('',*,*,#4930,.T.);
#6322=ORIENTED_EDGE('',*,*,#4925,.T.);
#6323=ORIENTED_EDGE('',*,*,#4922,.T.);
#6324=ORIENTED_EDGE('',*,*,#4919,.T.);
#6325=ORIENTED_EDGE('',*,*,#4916,.T.);
#6326=ORIENTED_EDGE('',*,*,#4934,.F.);
#6327=ORIENTED_EDGE('',*,*,#4926,.T.);
#6328=ORIENTED_EDGE('',*,*,#4923,.T.);
#6329=ORIENTED_EDGE('',*,*,#4920,.T.);
#6330=ORIENTED_EDGE('',*,*,#4917,.T.);
#6331=ORIENTED_EDGE('',*,*,#4914,.T.);
#6332=ORIENTED_EDGE('',*,*,#4935,.F.);
#6333=ORIENTED_EDGE('',*,*,#4936,.T.);
#6334=ORIENTED_EDGE('',*,*,#4937,.F.);
#6335=ORIENTED_EDGE('',*,*,#4936,.F.);
#6336=ORIENTED_EDGE('',*,*,#4938,.F.);
#6337=ORIENTED_EDGE('',*,*,#4939,.T.);
#6338=ORIENTED_EDGE('',*,*,#4940,.F.);
#6339=ORIENTED_EDGE('',*,*,#4939,.F.);
#6340=ORIENTED_EDGE('',*,*,#4941,.F.);
#6341=ORIENTED_EDGE('',*,*,#4942,.T.);
#6342=ORIENTED_EDGE('',*,*,#4943,.F.);
#6343=ORIENTED_EDGE('',*,*,#4942,.F.);
#6344=ORIENTED_EDGE('',*,*,#4944,.F.);
#6345=ORIENTED_EDGE('',*,*,#4945,.T.);
#6346=ORIENTED_EDGE('',*,*,#4946,.F.);
#6347=ORIENTED_EDGE('',*,*,#4945,.F.);
#6348=ORIENTED_EDGE('',*,*,#4947,.F.);
#6349=ORIENTED_EDGE('',*,*,#4948,.T.);
#6350=ORIENTED_EDGE('',*,*,#4949,.F.);
#6351=ORIENTED_EDGE('',*,*,#4948,.F.);
#6352=ORIENTED_EDGE('',*,*,#4950,.F.);
#6353=ORIENTED_EDGE('',*,*,#4951,.T.);
#6354=ORIENTED_EDGE('',*,*,#4952,.F.);
#6355=ORIENTED_EDGE('',*,*,#4951,.F.);
#6356=ORIENTED_EDGE('',*,*,#4953,.F.);
#6357=ORIENTED_EDGE('',*,*,#4954,.T.);
#6358=ORIENTED_EDGE('',*,*,#4955,.F.);
#6359=ORIENTED_EDGE('',*,*,#4954,.F.);
#6360=ORIENTED_EDGE('',*,*,#4956,.F.);
#6361=ORIENTED_EDGE('',*,*,#4957,.F.);
#6362=ORIENTED_EDGE('',*,*,#4958,.T.);
#6363=ORIENTED_EDGE('',*,*,#4959,.F.);
#6364=ORIENTED_EDGE('',*,*,#4955,.T.);
#6365=ORIENTED_EDGE('',*,*,#4960,.F.);
#6366=ORIENTED_EDGE('',*,*,#4961,.F.);
#6367=ORIENTED_EDGE('',*,*,#4962,.F.);
#6368=ORIENTED_EDGE('',*,*,#4963,.F.);
#6369=ORIENTED_EDGE('',*,*,#4952,.T.);
#6370=ORIENTED_EDGE('',*,*,#4964,.F.);
#6371=ORIENTED_EDGE('',*,*,#4962,.T.);
#6372=ORIENTED_EDGE('',*,*,#4965,.F.);
#6373=ORIENTED_EDGE('',*,*,#4966,.F.);
#6374=ORIENTED_EDGE('',*,*,#4967,.F.);
#6375=ORIENTED_EDGE('',*,*,#4968,.T.);
#6376=ORIENTED_EDGE('',*,*,#4969,.F.);
#6377=ORIENTED_EDGE('',*,*,#4958,.F.);
#6378=ORIENTED_EDGE('',*,*,#4970,.T.);
#6379=ORIENTED_EDGE('',*,*,#4971,.F.);
#6380=ORIENTED_EDGE('',*,*,#4972,.F.);
#6381=ORIENTED_EDGE('',*,*,#4963,.T.);
#6382=ORIENTED_EDGE('',*,*,#4964,.T.);
#6383=ORIENTED_EDGE('',*,*,#4973,.T.);
#6384=ORIENTED_EDGE('',*,*,#4967,.T.);
#6385=ORIENTED_EDGE('',*,*,#4957,.T.);
#6386=ORIENTED_EDGE('',*,*,#4956,.T.);
#6387=ORIENTED_EDGE('',*,*,#4974,.T.);
#6388=ORIENTED_EDGE('',*,*,#4975,.F.);
#6389=ORIENTED_EDGE('',*,*,#4970,.F.);
#6390=ORIENTED_EDGE('',*,*,#4949,.T.);
#6391=ORIENTED_EDGE('',*,*,#4946,.T.);
#6392=ORIENTED_EDGE('',*,*,#4943,.T.);
#6393=ORIENTED_EDGE('',*,*,#4940,.T.);
#6394=ORIENTED_EDGE('',*,*,#4937,.T.);
#6395=ORIENTED_EDGE('',*,*,#4976,.T.);
#6396=ORIENTED_EDGE('',*,*,#4977,.F.);
#6397=ORIENTED_EDGE('',*,*,#4974,.F.);
#6398=ORIENTED_EDGE('',*,*,#4959,.T.);
#6399=ORIENTED_EDGE('',*,*,#4969,.T.);
#6400=ORIENTED_EDGE('',*,*,#4978,.T.);
#6401=ORIENTED_EDGE('',*,*,#4965,.T.);
#6402=ORIENTED_EDGE('',*,*,#4961,.T.);
#6403=ORIENTED_EDGE('',*,*,#4960,.T.);
#6404=ORIENTED_EDGE('',*,*,#4972,.T.);
#6405=ORIENTED_EDGE('',*,*,#4979,.F.);
#6406=ORIENTED_EDGE('',*,*,#4976,.F.);
#6407=ORIENTED_EDGE('',*,*,#4947,.T.);
#6408=ORIENTED_EDGE('',*,*,#4944,.T.);
#6409=ORIENTED_EDGE('',*,*,#4941,.T.);
#6410=ORIENTED_EDGE('',*,*,#4938,.T.);
#6411=ORIENTED_EDGE('',*,*,#4935,.T.);
#6412=ORIENTED_EDGE('',*,*,#4979,.T.);
#6413=ORIENTED_EDGE('',*,*,#4971,.T.);
#6414=ORIENTED_EDGE('',*,*,#4975,.T.);
#6415=ORIENTED_EDGE('',*,*,#4977,.T.);
#6416=ORIENTED_EDGE('',*,*,#4978,.F.);
#6417=ORIENTED_EDGE('',*,*,#4968,.F.);
#6418=ORIENTED_EDGE('',*,*,#4973,.F.);
#6419=ORIENTED_EDGE('',*,*,#4966,.T.);
#6420=ORIENTED_EDGE('',*,*,#4950,.T.);
#6421=ORIENTED_EDGE('',*,*,#4953,.T.);
#6422=ORIENTED_EDGE('',*,*,#4980,.F.);
#6423=ORIENTED_EDGE('',*,*,#4981,.T.);
#6424=ORIENTED_EDGE('',*,*,#4982,.F.);
#6425=ORIENTED_EDGE('',*,*,#4981,.F.);
#6426=ORIENTED_EDGE('',*,*,#4983,.F.);
#6427=ORIENTED_EDGE('',*,*,#4984,.T.);
#6428=ORIENTED_EDGE('',*,*,#4985,.F.);
#6429=ORIENTED_EDGE('',*,*,#4984,.F.);
#6430=ORIENTED_EDGE('',*,*,#4986,.F.);
#6431=ORIENTED_EDGE('',*,*,#4987,.T.);
#6432=ORIENTED_EDGE('',*,*,#4988,.F.);
#6433=ORIENTED_EDGE('',*,*,#4987,.F.);
#6434=ORIENTED_EDGE('',*,*,#4989,.F.);
#6435=ORIENTED_EDGE('',*,*,#4990,.T.);
#6436=ORIENTED_EDGE('',*,*,#4991,.F.);
#6437=ORIENTED_EDGE('',*,*,#4990,.F.);
#6438=ORIENTED_EDGE('',*,*,#4992,.F.);
#6439=ORIENTED_EDGE('',*,*,#4993,.T.);
#6440=ORIENTED_EDGE('',*,*,#4994,.F.);
#6441=ORIENTED_EDGE('',*,*,#4993,.F.);
#6442=ORIENTED_EDGE('',*,*,#4992,.T.);
#6443=ORIENTED_EDGE('',*,*,#4995,.T.);
#6444=ORIENTED_EDGE('',*,*,#4995,.F.);
#6445=ORIENTED_EDGE('',*,*,#4996,.T.);
#6446=ORIENTED_EDGE('',*,*,#4997,.T.);
#6447=ORIENTED_EDGE('',*,*,#4996,.F.);
#6448=ORIENTED_EDGE('',*,*,#4998,.F.);
#6449=ORIENTED_EDGE('',*,*,#4999,.T.);
#6450=ORIENTED_EDGE('',*,*,#5000,.T.);
#6451=ORIENTED_EDGE('',*,*,#4999,.F.);
#6452=ORIENTED_EDGE('',*,*,#4998,.T.);
#6453=ORIENTED_EDGE('',*,*,#4994,.T.);
#6454=ORIENTED_EDGE('',*,*,#4991,.T.);
#6455=ORIENTED_EDGE('',*,*,#4988,.T.);
#6456=ORIENTED_EDGE('',*,*,#4985,.T.);
#6457=ORIENTED_EDGE('',*,*,#4982,.T.);
#6458=ORIENTED_EDGE('',*,*,#5000,.F.);
#6459=ORIENTED_EDGE('',*,*,#4997,.F.);
#6460=ORIENTED_EDGE('',*,*,#4989,.T.);
#6461=ORIENTED_EDGE('',*,*,#4986,.T.);
#6462=ORIENTED_EDGE('',*,*,#4983,.T.);
#6463=ORIENTED_EDGE('',*,*,#4980,.T.);
#6464=ORIENTED_EDGE('',*,*,#5001,.F.);
#6465=ORIENTED_EDGE('',*,*,#5002,.T.);
#6466=ORIENTED_EDGE('',*,*,#5003,.F.);
#6467=ORIENTED_EDGE('',*,*,#5002,.F.);
#6468=ORIENTED_EDGE('',*,*,#5004,.F.);
#6469=ORIENTED_EDGE('',*,*,#5005,.T.);
#6470=ORIENTED_EDGE('',*,*,#5006,.F.);
#6471=ORIENTED_EDGE('',*,*,#5005,.F.);
#6472=ORIENTED_EDGE('',*,*,#5007,.F.);
#6473=ORIENTED_EDGE('',*,*,#5008,.T.);
#6474=ORIENTED_EDGE('',*,*,#5009,.F.);
#6475=ORIENTED_EDGE('',*,*,#5008,.F.);
#6476=ORIENTED_EDGE('',*,*,#5010,.F.);
#6477=ORIENTED_EDGE('',*,*,#5011,.T.);
#6478=ORIENTED_EDGE('',*,*,#5012,.F.);
#6479=ORIENTED_EDGE('',*,*,#5011,.F.);
#6480=ORIENTED_EDGE('',*,*,#5013,.F.);
#6481=ORIENTED_EDGE('',*,*,#5014,.T.);
#6482=ORIENTED_EDGE('',*,*,#5015,.T.);
#6483=ORIENTED_EDGE('',*,*,#5014,.F.);
#6484=ORIENTED_EDGE('',*,*,#5015,.F.);
#6485=ORIENTED_EDGE('',*,*,#5016,.F.);
#6486=ORIENTED_EDGE('',*,*,#5017,.F.);
#6487=ORIENTED_EDGE('',*,*,#5018,.T.);
#6488=ORIENTED_EDGE('',*,*,#5016,.T.);
#6489=ORIENTED_EDGE('',*,*,#5018,.F.);
#6490=ORIENTED_EDGE('',*,*,#5019,.F.);
#6491=ORIENTED_EDGE('',*,*,#5020,.T.);
#6492=ORIENTED_EDGE('',*,*,#5021,.T.);
#6493=ORIENTED_EDGE('',*,*,#5020,.F.);
#6494=ORIENTED_EDGE('',*,*,#5019,.T.);
#6495=ORIENTED_EDGE('',*,*,#5017,.T.);
#6496=ORIENTED_EDGE('',*,*,#5012,.T.);
#6497=ORIENTED_EDGE('',*,*,#5009,.T.);
#6498=ORIENTED_EDGE('',*,*,#5006,.T.);
#6499=ORIENTED_EDGE('',*,*,#5003,.T.);
#6500=ORIENTED_EDGE('',*,*,#5021,.F.);
#6501=ORIENTED_EDGE('',*,*,#5013,.T.);
#6502=ORIENTED_EDGE('',*,*,#5010,.T.);
#6503=ORIENTED_EDGE('',*,*,#5007,.T.);
#6504=ORIENTED_EDGE('',*,*,#5004,.T.);
#6505=ORIENTED_EDGE('',*,*,#5001,.T.);
#6506=ORIENTED_EDGE('',*,*,#5022,.F.);
#6507=ORIENTED_EDGE('',*,*,#5023,.T.);
#6508=ORIENTED_EDGE('',*,*,#5024,.F.);
#6509=ORIENTED_EDGE('',*,*,#5023,.F.);
#6510=ORIENTED_EDGE('',*,*,#5025,.F.);
#6511=ORIENTED_EDGE('',*,*,#5026,.T.);
#6512=ORIENTED_EDGE('',*,*,#5027,.F.);
#6513=ORIENTED_EDGE('',*,*,#5026,.F.);
#6514=ORIENTED_EDGE('',*,*,#5028,.F.);
#6515=ORIENTED_EDGE('',*,*,#5029,.T.);
#6516=ORIENTED_EDGE('',*,*,#5030,.F.);
#6517=ORIENTED_EDGE('',*,*,#5029,.F.);
#6518=ORIENTED_EDGE('',*,*,#5028,.T.);
#6519=ORIENTED_EDGE('',*,*,#5031,.F.);
#6520=ORIENTED_EDGE('',*,*,#5032,.F.);
#6521=ORIENTED_EDGE('',*,*,#5033,.T.);
#6522=ORIENTED_EDGE('',*,*,#5031,.T.);
#6523=ORIENTED_EDGE('',*,*,#5033,.F.);
#6524=ORIENTED_EDGE('',*,*,#5034,.F.);
#6525=ORIENTED_EDGE('',*,*,#5035,.T.);
#6526=ORIENTED_EDGE('',*,*,#5036,.F.);
#6527=ORIENTED_EDGE('',*,*,#5035,.F.);
#6528=ORIENTED_EDGE('',*,*,#5034,.T.);
#6529=ORIENTED_EDGE('',*,*,#5037,.F.);
#6530=ORIENTED_EDGE('',*,*,#5038,.F.);
#6531=ORIENTED_EDGE('',*,*,#5039,.T.);
#6532=ORIENTED_EDGE('',*,*,#5037,.T.);
#6533=ORIENTED_EDGE('',*,*,#5039,.F.);
#6534=ORIENTED_EDGE('',*,*,#5040,.T.);
#6535=ORIENTED_EDGE('',*,*,#5041,.T.);
#6536=ORIENTED_EDGE('',*,*,#5042,.F.);
#6537=ORIENTED_EDGE('',*,*,#5043,.F.);
#6538=ORIENTED_EDGE('',*,*,#5024,.T.);
#6539=ORIENTED_EDGE('',*,*,#5027,.T.);
#6540=ORIENTED_EDGE('',*,*,#5044,.T.);
#6541=ORIENTED_EDGE('',*,*,#5043,.T.);
#6542=ORIENTED_EDGE('',*,*,#5045,.F.);
#6543=ORIENTED_EDGE('',*,*,#5046,.F.);
#6544=ORIENTED_EDGE('',*,*,#5047,.T.);
#6545=ORIENTED_EDGE('',*,*,#5046,.T.);
#6546=ORIENTED_EDGE('',*,*,#5048,.F.);
#6547=ORIENTED_EDGE('',*,*,#5049,.F.);
#6548=ORIENTED_EDGE('',*,*,#5022,.T.);
#6549=ORIENTED_EDGE('',*,*,#5025,.T.);
#6550=ORIENTED_EDGE('',*,*,#5050,.T.);
#6551=ORIENTED_EDGE('',*,*,#5049,.T.);
#6552=ORIENTED_EDGE('',*,*,#5051,.F.);
#6553=ORIENTED_EDGE('',*,*,#5041,.F.);
#6554=ORIENTED_EDGE('',*,*,#5051,.T.);
#6555=ORIENTED_EDGE('',*,*,#5048,.T.);
#6556=ORIENTED_EDGE('',*,*,#5045,.T.);
#6557=ORIENTED_EDGE('',*,*,#5042,.T.);
#6558=ORIENTED_EDGE('',*,*,#5030,.T.);
#6559=ORIENTED_EDGE('',*,*,#5036,.T.);
#6560=ORIENTED_EDGE('',*,*,#5050,.F.);
#6561=ORIENTED_EDGE('',*,*,#5040,.F.);
#6562=ORIENTED_EDGE('',*,*,#5044,.F.);
#6563=ORIENTED_EDGE('',*,*,#5047,.F.);
#6564=ORIENTED_EDGE('',*,*,#5032,.T.);
#6565=ORIENTED_EDGE('',*,*,#5038,.T.);
#6566=ORIENTED_EDGE('',*,*,#5052,.F.);
#6567=ORIENTED_EDGE('',*,*,#5053,.T.);
#6568=ORIENTED_EDGE('',*,*,#5054,.T.);
#6569=ORIENTED_EDGE('',*,*,#5053,.F.);
#6570=ORIENTED_EDGE('',*,*,#5052,.T.);
#6571=ORIENTED_EDGE('',*,*,#5054,.F.);
#6572=ORIENTED_EDGE('',*,*,#5055,.F.);
#6573=ORIENTED_EDGE('',*,*,#5056,.T.);
#6574=ORIENTED_EDGE('',*,*,#5057,.T.);
#6575=ORIENTED_EDGE('',*,*,#5056,.F.);
#6576=ORIENTED_EDGE('',*,*,#5055,.T.);
#6577=ORIENTED_EDGE('',*,*,#5057,.F.);
#6578=ORIENTED_EDGE('',*,*,#5058,.T.);
#6579=ORIENTED_EDGE('',*,*,#5059,.T.);
#6580=ORIENTED_EDGE('',*,*,#5060,.F.);
#6581=ORIENTED_EDGE('',*,*,#5059,.F.);
#6582=ORIENTED_EDGE('',*,*,#5060,.T.);
#6583=ORIENTED_EDGE('',*,*,#5058,.F.);
#6584=ORIENTED_EDGE('',*,*,#5061,.F.);
#6585=ORIENTED_EDGE('',*,*,#5062,.T.);
#6586=ORIENTED_EDGE('',*,*,#5063,.T.);
#6587=ORIENTED_EDGE('',*,*,#5062,.F.);
#6588=ORIENTED_EDGE('',*,*,#5061,.T.);
#6589=ORIENTED_EDGE('',*,*,#5063,.F.);
#6590=ORIENTED_EDGE('',*,*,#5064,.F.);
#6591=ORIENTED_EDGE('',*,*,#5065,.T.);
#6592=ORIENTED_EDGE('',*,*,#5066,.T.);
#6593=ORIENTED_EDGE('',*,*,#5065,.F.);
#6594=ORIENTED_EDGE('',*,*,#5064,.T.);
#6595=ORIENTED_EDGE('',*,*,#5066,.F.);
#6596=ORIENTED_EDGE('',*,*,#5067,.T.);
#6597=ORIENTED_EDGE('',*,*,#5068,.T.);
#6598=ORIENTED_EDGE('',*,*,#5069,.F.);
#6599=ORIENTED_EDGE('',*,*,#5068,.F.);
#6600=ORIENTED_EDGE('',*,*,#5069,.T.);
#6601=ORIENTED_EDGE('',*,*,#5067,.F.);
#6602=ORIENTED_EDGE('',*,*,#5070,.F.);
#6603=ORIENTED_EDGE('',*,*,#5071,.F.);
#6604=ORIENTED_EDGE('',*,*,#5072,.T.);
#6605=ORIENTED_EDGE('',*,*,#5070,.T.);
#6606=ORIENTED_EDGE('',*,*,#5072,.F.);
#6607=ORIENTED_EDGE('',*,*,#5073,.F.);
#6608=ORIENTED_EDGE('',*,*,#5074,.T.);
#6609=ORIENTED_EDGE('',*,*,#5071,.T.);
#6610=ORIENTED_EDGE('',*,*,#5074,.F.);
#6611=ORIENTED_EDGE('',*,*,#5075,.F.);
#6612=ORIENTED_EDGE('',*,*,#5076,.T.);
#6613=ORIENTED_EDGE('',*,*,#5073,.T.);
#6614=ORIENTED_EDGE('',*,*,#5076,.F.);
#6615=ORIENTED_EDGE('',*,*,#5075,.T.);
#6616=ORIENTED_EDGE('',*,*,#5077,.F.);
#6617=ORIENTED_EDGE('',*,*,#5078,.F.);
#6618=ORIENTED_EDGE('',*,*,#5079,.T.);
#6619=ORIENTED_EDGE('',*,*,#5077,.T.);
#6620=ORIENTED_EDGE('',*,*,#5079,.F.);
#6621=ORIENTED_EDGE('',*,*,#5080,.F.);
#6622=ORIENTED_EDGE('',*,*,#5081,.T.);
#6623=ORIENTED_EDGE('',*,*,#5078,.T.);
#6624=ORIENTED_EDGE('',*,*,#5081,.F.);
#6625=ORIENTED_EDGE('',*,*,#5082,.F.);
#6626=ORIENTED_EDGE('',*,*,#5083,.T.);
#6627=ORIENTED_EDGE('',*,*,#5080,.T.);
#6628=ORIENTED_EDGE('',*,*,#5083,.F.);
#6629=ORIENTED_EDGE('',*,*,#5082,.T.);
#6630=ORIENTED_EDGE('',*,*,#5084,.T.);
#6631=ORIENTED_EDGE('',*,*,#5085,.T.);
#6632=ORIENTED_EDGE('',*,*,#5086,.T.);
#6633=ORIENTED_EDGE('',*,*,#5087,.F.);
#6634=ORIENTED_EDGE('',*,*,#5088,.T.);
#6635=ORIENTED_EDGE('',*,*,#5089,.T.);
#6636=ORIENTED_EDGE('',*,*,#5090,.T.);
#6637=ORIENTED_EDGE('',*,*,#5085,.F.);
#6638=ORIENTED_EDGE('',*,*,#5091,.T.);
#6639=ORIENTED_EDGE('',*,*,#5092,.T.);
#6640=ORIENTED_EDGE('',*,*,#5093,.T.);
#6641=ORIENTED_EDGE('',*,*,#5089,.F.);
#6642=ORIENTED_EDGE('',*,*,#5094,.T.);
#6643=ORIENTED_EDGE('',*,*,#5095,.T.);
#6644=ORIENTED_EDGE('',*,*,#5096,.T.);
#6645=ORIENTED_EDGE('',*,*,#5092,.F.);
#6646=ORIENTED_EDGE('',*,*,#5097,.T.);
#6647=ORIENTED_EDGE('',*,*,#5098,.T.);
#6648=ORIENTED_EDGE('',*,*,#5099,.T.);
#6649=ORIENTED_EDGE('',*,*,#5095,.F.);
#6650=ORIENTED_EDGE('',*,*,#5100,.T.);
#6651=ORIENTED_EDGE('',*,*,#5087,.T.);
#6652=ORIENTED_EDGE('',*,*,#5101,.T.);
#6653=ORIENTED_EDGE('',*,*,#5098,.F.);
#6654=ORIENTED_EDGE('',*,*,#5100,.F.);
#6655=ORIENTED_EDGE('',*,*,#5097,.F.);
#6656=ORIENTED_EDGE('',*,*,#5094,.F.);
#6657=ORIENTED_EDGE('',*,*,#5091,.F.);
#6658=ORIENTED_EDGE('',*,*,#5088,.F.);
#6659=ORIENTED_EDGE('',*,*,#5084,.F.);
#6660=ORIENTED_EDGE('',*,*,#5101,.F.);
#6661=ORIENTED_EDGE('',*,*,#5086,.F.);
#6662=ORIENTED_EDGE('',*,*,#5090,.F.);
#6663=ORIENTED_EDGE('',*,*,#5093,.F.);
#6664=ORIENTED_EDGE('',*,*,#5096,.F.);
#6665=ORIENTED_EDGE('',*,*,#5099,.F.);
#6666=ORIENTED_EDGE('',*,*,#5102,.F.);
#6667=ORIENTED_EDGE('',*,*,#5103,.F.);
#6668=ORIENTED_EDGE('',*,*,#5104,.T.);
#6669=ORIENTED_EDGE('',*,*,#5105,.F.);
#6670=ORIENTED_EDGE('',*,*,#5106,.F.);
#6671=ORIENTED_EDGE('',*,*,#5104,.F.);
#6672=ORIENTED_EDGE('',*,*,#5105,.T.);
#6673=ORIENTED_EDGE('',*,*,#5106,.T.);
#6674=ORIENTED_EDGE('',*,*,#5107,.T.);
#6675=ORIENTED_EDGE('',*,*,#5108,.T.);
#6676=ORIENTED_EDGE('',*,*,#5107,.F.);
#6677=ORIENTED_EDGE('',*,*,#5109,.T.);
#6678=ORIENTED_EDGE('',*,*,#5110,.T.);
#6679=ORIENTED_EDGE('',*,*,#5111,.F.);
#6680=ORIENTED_EDGE('',*,*,#5110,.F.);
#6681=ORIENTED_EDGE('',*,*,#5111,.T.);
#6682=ORIENTED_EDGE('',*,*,#5112,.T.);
#6683=ORIENTED_EDGE('',*,*,#5113,.F.);
#6684=ORIENTED_EDGE('',*,*,#5112,.F.);
#6685=ORIENTED_EDGE('',*,*,#5108,.F.);
#6686=ORIENTED_EDGE('',*,*,#5113,.T.);
#6687=ORIENTED_EDGE('',*,*,#5114,.F.);
#6688=ORIENTED_EDGE('',*,*,#5115,.T.);
#6689=ORIENTED_EDGE('',*,*,#5102,.T.);
#6690=ORIENTED_EDGE('',*,*,#5103,.T.);
#6691=ORIENTED_EDGE('',*,*,#5115,.F.);
#6692=ORIENTED_EDGE('',*,*,#5114,.T.);
#6693=ORIENTED_EDGE('',*,*,#5116,.F.);
#6694=ORIENTED_EDGE('',*,*,#5116,.T.);
#6695=ORIENTED_EDGE('',*,*,#5117,.T.);
#6696=ORIENTED_EDGE('',*,*,#5109,.F.);
#6697=ORIENTED_EDGE('',*,*,#5117,.F.);
#6698=ORIENTED_EDGE('',*,*,#5118,.F.);
#6699=ORIENTED_EDGE('',*,*,#5119,.F.);
#6700=ORIENTED_EDGE('',*,*,#5120,.T.);
#6701=ORIENTED_EDGE('',*,*,#5121,.F.);
#6702=ORIENTED_EDGE('',*,*,#5122,.F.);
#6703=ORIENTED_EDGE('',*,*,#5120,.F.);
#6704=ORIENTED_EDGE('',*,*,#5123,.T.);
#6705=ORIENTED_EDGE('',*,*,#5124,.T.);
#6706=ORIENTED_EDGE('',*,*,#5121,.T.);
#6707=ORIENTED_EDGE('',*,*,#5122,.T.);
#6708=ORIENTED_EDGE('',*,*,#5124,.F.);
#6709=ORIENTED_EDGE('',*,*,#5125,.F.);
#6710=ORIENTED_EDGE('',*,*,#5126,.T.);
#6711=ORIENTED_EDGE('',*,*,#5127,.F.);
#6712=ORIENTED_EDGE('',*,*,#5128,.T.);
#6713=ORIENTED_EDGE('',*,*,#5125,.T.);
#6714=ORIENTED_EDGE('',*,*,#5128,.F.);
#6715=ORIENTED_EDGE('',*,*,#5129,.F.);
#6716=ORIENTED_EDGE('',*,*,#5130,.T.);
#6717=ORIENTED_EDGE('',*,*,#5127,.T.);
#6718=ORIENTED_EDGE('',*,*,#5130,.F.);
#6719=ORIENTED_EDGE('',*,*,#5131,.F.);
#6720=ORIENTED_EDGE('',*,*,#5132,.T.);
#6721=ORIENTED_EDGE('',*,*,#5129,.T.);
#6722=ORIENTED_EDGE('',*,*,#5132,.F.);
#6723=ORIENTED_EDGE('',*,*,#5131,.T.);
#6724=ORIENTED_EDGE('',*,*,#5123,.F.);
#6725=ORIENTED_EDGE('',*,*,#5118,.T.);
#6726=ORIENTED_EDGE('',*,*,#5119,.T.);
#6727=ORIENTED_EDGE('',*,*,#5133,.T.);
#6728=ORIENTED_EDGE('',*,*,#5126,.F.);
#6729=ORIENTED_EDGE('',*,*,#5133,.F.);
#6730=ORIENTED_EDGE('',*,*,#5134,.T.);
#6731=ORIENTED_EDGE('',*,*,#5134,.F.);
#6732=ORIENTED_EDGE('',*,*,#5135,.T.);
#6733=ORIENTED_EDGE('',*,*,#5135,.F.);
#6734=ORIENTED_EDGE('',*,*,#5136,.T.);
#6735=ORIENTED_EDGE('',*,*,#5136,.F.);
#6736=ORIENTED_EDGE('',*,*,#5137,.T.);
#6737=ORIENTED_EDGE('',*,*,#5137,.F.);
#6738=ORIENTED_EDGE('',*,*,#5138,.T.);
#6739=ORIENTED_EDGE('',*,*,#5138,.F.);
#6740=ORIENTED_EDGE('',*,*,#5139,.T.);
#6741=ORIENTED_EDGE('',*,*,#5139,.F.);
#6742=ORIENTED_EDGE('',*,*,#5140,.T.);
#6743=ORIENTED_EDGE('',*,*,#5140,.F.);
#6744=ORIENTED_EDGE('',*,*,#5141,.F.);
#6745=ORIENTED_EDGE('',*,*,#5142,.F.);
#6746=ORIENTED_EDGE('',*,*,#5143,.F.);
#6747=ORIENTED_EDGE('',*,*,#5144,.F.);
#6748=ORIENTED_EDGE('',*,*,#5143,.T.);
#6749=ORIENTED_EDGE('',*,*,#5145,.F.);
#6750=ORIENTED_EDGE('',*,*,#5146,.T.);
#6751=ORIENTED_EDGE('',*,*,#5147,.F.);
#6752=ORIENTED_EDGE('',*,*,#5148,.T.);
#6753=ORIENTED_EDGE('',*,*,#5149,.F.);
#6754=ORIENTED_EDGE('',*,*,#5150,.T.);
#6755=ORIENTED_EDGE('',*,*,#5151,.F.);
#6756=ORIENTED_EDGE('',*,*,#5150,.F.);
#6757=ORIENTED_EDGE('',*,*,#5152,.F.);
#6758=ORIENTED_EDGE('',*,*,#5153,.T.);
#6759=ORIENTED_EDGE('',*,*,#5154,.F.);
#6760=ORIENTED_EDGE('',*,*,#5155,.T.);
#6761=ORIENTED_EDGE('',*,*,#5156,.F.);
#6762=ORIENTED_EDGE('',*,*,#5157,.T.);
#6763=ORIENTED_EDGE('',*,*,#5158,.F.);
#6764=ORIENTED_EDGE('',*,*,#5159,.T.);
#6765=ORIENTED_EDGE('',*,*,#5160,.F.);
#6766=ORIENTED_EDGE('',*,*,#5142,.T.);
#6767=ORIENTED_EDGE('',*,*,#5161,.T.);
#6768=ORIENTED_EDGE('',*,*,#5162,.T.);
#6769=ORIENTED_EDGE('',*,*,#5145,.T.);
#6770=ORIENTED_EDGE('',*,*,#5163,.F.);
#6771=ORIENTED_EDGE('',*,*,#5164,.F.);
#6772=ORIENTED_EDGE('',*,*,#5146,.F.);
#6773=ORIENTED_EDGE('',*,*,#5162,.F.);
#6774=ORIENTED_EDGE('',*,*,#5164,.T.);
#6775=ORIENTED_EDGE('',*,*,#5165,.T.);
#6776=ORIENTED_EDGE('',*,*,#5166,.T.);
#6777=ORIENTED_EDGE('',*,*,#5147,.T.);
#6778=ORIENTED_EDGE('',*,*,#5167,.F.);
#6779=ORIENTED_EDGE('',*,*,#5168,.F.);
#6780=ORIENTED_EDGE('',*,*,#5148,.F.);
#6781=ORIENTED_EDGE('',*,*,#5166,.F.);
#6782=ORIENTED_EDGE('',*,*,#5168,.T.);
#6783=ORIENTED_EDGE('',*,*,#5169,.T.);
#6784=ORIENTED_EDGE('',*,*,#5170,.T.);
#6785=ORIENTED_EDGE('',*,*,#5171,.T.);
#6786=ORIENTED_EDGE('',*,*,#5152,.T.);
#6787=ORIENTED_EDGE('',*,*,#5149,.T.);
#6788=ORIENTED_EDGE('',*,*,#5172,.F.);
#6789=ORIENTED_EDGE('',*,*,#5173,.F.);
#6790=ORIENTED_EDGE('',*,*,#5153,.F.);
#6791=ORIENTED_EDGE('',*,*,#5171,.F.);
#6792=ORIENTED_EDGE('',*,*,#5173,.T.);
#6793=ORIENTED_EDGE('',*,*,#5174,.T.);
#6794=ORIENTED_EDGE('',*,*,#5175,.T.);
#6795=ORIENTED_EDGE('',*,*,#5154,.T.);
#6796=ORIENTED_EDGE('',*,*,#5176,.F.);
#6797=ORIENTED_EDGE('',*,*,#5177,.F.);
#6798=ORIENTED_EDGE('',*,*,#5155,.F.);
#6799=ORIENTED_EDGE('',*,*,#5175,.F.);
#6800=ORIENTED_EDGE('',*,*,#5177,.T.);
#6801=ORIENTED_EDGE('',*,*,#5178,.T.);
#6802=ORIENTED_EDGE('',*,*,#5179,.T.);
#6803=ORIENTED_EDGE('',*,*,#5156,.T.);
#6804=ORIENTED_EDGE('',*,*,#5157,.F.);
#6805=ORIENTED_EDGE('',*,*,#5179,.F.);
#6806=ORIENTED_EDGE('',*,*,#5180,.F.);
#6807=ORIENTED_EDGE('',*,*,#5181,.F.);
#6808=ORIENTED_EDGE('',*,*,#5182,.F.);
#6809=ORIENTED_EDGE('',*,*,#5183,.T.);
#6810=ORIENTED_EDGE('',*,*,#5169,.F.);
#6811=ORIENTED_EDGE('',*,*,#5167,.T.);
#6812=ORIENTED_EDGE('',*,*,#5165,.F.);
#6813=ORIENTED_EDGE('',*,*,#5163,.T.);
#6814=ORIENTED_EDGE('',*,*,#5161,.F.);
#6815=ORIENTED_EDGE('',*,*,#5141,.T.);
#6816=ORIENTED_EDGE('',*,*,#5184,.F.);
#6817=ORIENTED_EDGE('',*,*,#5185,.T.);
#6818=ORIENTED_EDGE('',*,*,#5186,.F.);
#6819=ORIENTED_EDGE('',*,*,#5180,.T.);
#6820=ORIENTED_EDGE('',*,*,#5178,.F.);
#6821=ORIENTED_EDGE('',*,*,#5176,.T.);
#6822=ORIENTED_EDGE('',*,*,#5174,.F.);
#6823=ORIENTED_EDGE('',*,*,#5172,.T.);
#6824=ORIENTED_EDGE('',*,*,#5170,.F.);
#6825=ORIENTED_EDGE('',*,*,#5183,.F.);
#6826=ORIENTED_EDGE('',*,*,#5144,.T.);
#6827=ORIENTED_EDGE('',*,*,#5160,.T.);
#6828=ORIENTED_EDGE('',*,*,#5187,.T.);
#6829=ORIENTED_EDGE('',*,*,#5184,.T.);
#6830=ORIENTED_EDGE('',*,*,#5159,.F.);
#6831=ORIENTED_EDGE('',*,*,#5188,.F.);
#6832=ORIENTED_EDGE('',*,*,#5185,.F.);
#6833=ORIENTED_EDGE('',*,*,#5187,.F.);
#6834=ORIENTED_EDGE('',*,*,#5151,.T.);
#6835=ORIENTED_EDGE('',*,*,#5182,.T.);
#6836=ORIENTED_EDGE('',*,*,#5181,.T.);
#6837=ORIENTED_EDGE('',*,*,#5186,.T.);
#6838=ORIENTED_EDGE('',*,*,#5188,.T.);
#6839=ORIENTED_EDGE('',*,*,#5158,.T.);
#6840=ORIENTED_EDGE('',*,*,#5189,.F.);
#6841=ORIENTED_EDGE('',*,*,#5190,.T.);
#6842=ORIENTED_EDGE('',*,*,#5191,.F.);
#6843=ORIENTED_EDGE('',*,*,#5192,.T.);
#6844=ORIENTED_EDGE('',*,*,#5189,.T.);
#6845=ORIENTED_EDGE('',*,*,#5192,.F.);
#6846=ORIENTED_EDGE('',*,*,#5191,.T.);
#6847=ORIENTED_EDGE('',*,*,#5193,.F.);
#6848=ORIENTED_EDGE('',*,*,#5193,.T.);
#6849=ORIENTED_EDGE('',*,*,#5194,.T.);
#6850=ORIENTED_EDGE('',*,*,#5190,.F.);
#6851=ORIENTED_EDGE('',*,*,#5194,.F.);
#6852=ORIENTED_EDGE('',*,*,#5195,.F.);
#6853=ORIENTED_EDGE('',*,*,#5196,.T.);
#6854=ORIENTED_EDGE('',*,*,#5197,.F.);
#6855=ORIENTED_EDGE('',*,*,#5198,.T.);
#6856=ORIENTED_EDGE('',*,*,#5195,.T.);
#6857=ORIENTED_EDGE('',*,*,#5198,.F.);
#6858=ORIENTED_EDGE('',*,*,#5197,.T.);
#6859=ORIENTED_EDGE('',*,*,#5199,.F.);
#6860=ORIENTED_EDGE('',*,*,#5199,.T.);
#6861=ORIENTED_EDGE('',*,*,#5200,.T.);
#6862=ORIENTED_EDGE('',*,*,#5196,.F.);
#6863=ORIENTED_EDGE('',*,*,#5200,.F.);
#6864=ORIENTED_EDGE('',*,*,#5201,.T.);
#6865=ORIENTED_EDGE('',*,*,#5202,.T.);
#6866=ORIENTED_EDGE('',*,*,#5203,.T.);
#6867=ORIENTED_EDGE('',*,*,#5204,.F.);
#6868=ORIENTED_EDGE('',*,*,#5205,.T.);
#6869=ORIENTED_EDGE('',*,*,#5206,.T.);
#6870=ORIENTED_EDGE('',*,*,#5207,.T.);
#6871=ORIENTED_EDGE('',*,*,#5202,.F.);
#6872=ORIENTED_EDGE('',*,*,#5208,.T.);
#6873=ORIENTED_EDGE('',*,*,#5209,.T.);
#6874=ORIENTED_EDGE('',*,*,#5210,.T.);
#6875=ORIENTED_EDGE('',*,*,#5206,.F.);
#6876=ORIENTED_EDGE('',*,*,#5211,.T.);
#6877=ORIENTED_EDGE('',*,*,#5212,.T.);
#6878=ORIENTED_EDGE('',*,*,#5213,.T.);
#6879=ORIENTED_EDGE('',*,*,#5209,.F.);
#6880=ORIENTED_EDGE('',*,*,#5214,.T.);
#6881=ORIENTED_EDGE('',*,*,#5215,.T.);
#6882=ORIENTED_EDGE('',*,*,#5216,.T.);
#6883=ORIENTED_EDGE('',*,*,#5212,.F.);
#6884=ORIENTED_EDGE('',*,*,#5217,.T.);
#6885=ORIENTED_EDGE('',*,*,#5204,.T.);
#6886=ORIENTED_EDGE('',*,*,#5218,.T.);
#6887=ORIENTED_EDGE('',*,*,#5215,.F.);
#6888=ORIENTED_EDGE('',*,*,#5217,.F.);
#6889=ORIENTED_EDGE('',*,*,#5214,.F.);
#6890=ORIENTED_EDGE('',*,*,#5211,.F.);
#6891=ORIENTED_EDGE('',*,*,#5208,.F.);
#6892=ORIENTED_EDGE('',*,*,#5205,.F.);
#6893=ORIENTED_EDGE('',*,*,#5201,.F.);
#6894=ORIENTED_EDGE('',*,*,#5218,.F.);
#6895=ORIENTED_EDGE('',*,*,#5203,.F.);
#6896=ORIENTED_EDGE('',*,*,#5207,.F.);
#6897=ORIENTED_EDGE('',*,*,#5210,.F.);
#6898=ORIENTED_EDGE('',*,*,#5213,.F.);
#6899=ORIENTED_EDGE('',*,*,#5216,.F.);
#6900=ORIENTED_EDGE('',*,*,#5219,.F.);
#6901=ORIENTED_EDGE('',*,*,#5220,.F.);
#6902=ORIENTED_EDGE('',*,*,#5221,.F.);
#6903=ORIENTED_EDGE('',*,*,#5222,.T.);
#6904=ORIENTED_EDGE('',*,*,#5220,.T.);
#6905=ORIENTED_EDGE('',*,*,#5222,.F.);
#6906=ORIENTED_EDGE('',*,*,#5223,.F.);
#6907=ORIENTED_EDGE('',*,*,#5224,.T.);
#6908=ORIENTED_EDGE('',*,*,#5221,.T.);
#6909=ORIENTED_EDGE('',*,*,#5224,.F.);
#6910=ORIENTED_EDGE('',*,*,#5225,.F.);
#6911=ORIENTED_EDGE('',*,*,#5226,.T.);
#6912=ORIENTED_EDGE('',*,*,#5223,.T.);
#6913=ORIENTED_EDGE('',*,*,#5226,.F.);
#6914=ORIENTED_EDGE('',*,*,#5225,.T.);
#6915=ORIENTED_EDGE('',*,*,#5227,.F.);
#6916=ORIENTED_EDGE('',*,*,#5228,.F.);
#6917=ORIENTED_EDGE('',*,*,#5229,.T.);
#6918=ORIENTED_EDGE('',*,*,#5227,.T.);
#6919=ORIENTED_EDGE('',*,*,#5229,.F.);
#6920=ORIENTED_EDGE('',*,*,#5219,.T.);
#6921=ORIENTED_EDGE('',*,*,#5230,.T.);
#6922=ORIENTED_EDGE('',*,*,#5228,.T.);
#6923=ORIENTED_EDGE('',*,*,#5230,.F.);
#6924=ORIENTED_EDGE('',*,*,#5231,.F.);
#6925=ORIENTED_EDGE('',*,*,#5232,.F.);
#6926=ORIENTED_EDGE('',*,*,#5233,.T.);
#6927=ORIENTED_EDGE('',*,*,#5231,.T.);
#6928=ORIENTED_EDGE('',*,*,#5233,.F.);
#6929=ORIENTED_EDGE('',*,*,#5234,.F.);
#6930=ORIENTED_EDGE('',*,*,#5235,.T.);
#6931=ORIENTED_EDGE('',*,*,#5232,.T.);
#6932=ORIENTED_EDGE('',*,*,#5235,.F.);
#6933=ORIENTED_EDGE('',*,*,#5236,.F.);
#6934=ORIENTED_EDGE('',*,*,#5237,.T.);
#6935=ORIENTED_EDGE('',*,*,#5234,.T.);
#6936=ORIENTED_EDGE('',*,*,#5237,.F.);
#6937=ORIENTED_EDGE('',*,*,#5236,.T.);
#6938=ORIENTED_EDGE('',*,*,#5238,.F.);
#6939=ORIENTED_EDGE('',*,*,#5239,.F.);
#6940=ORIENTED_EDGE('',*,*,#5240,.T.);
#6941=ORIENTED_EDGE('',*,*,#5238,.T.);
#6942=ORIENTED_EDGE('',*,*,#5240,.F.);
#6943=ORIENTED_EDGE('',*,*,#5241,.F.);
#6944=ORIENTED_EDGE('',*,*,#5242,.T.);
#6945=ORIENTED_EDGE('',*,*,#5239,.T.);
#6946=ORIENTED_EDGE('',*,*,#5242,.F.);
#6947=ORIENTED_EDGE('',*,*,#5243,.F.);
#6948=ORIENTED_EDGE('',*,*,#5244,.T.);
#6949=ORIENTED_EDGE('',*,*,#5241,.T.);
#6950=ORIENTED_EDGE('',*,*,#5244,.F.);
#6951=ORIENTED_EDGE('',*,*,#5243,.T.);
#6952=ORIENTED_EDGE('',*,*,#5245,.T.);
#6953=ORIENTED_EDGE('',*,*,#5246,.T.);
#6954=ORIENTED_EDGE('',*,*,#5247,.T.);
#6955=ORIENTED_EDGE('',*,*,#5248,.F.);
#6956=ORIENTED_EDGE('',*,*,#5249,.T.);
#6957=ORIENTED_EDGE('',*,*,#5250,.T.);
#6958=ORIENTED_EDGE('',*,*,#5251,.T.);
#6959=ORIENTED_EDGE('',*,*,#5246,.F.);
#6960=ORIENTED_EDGE('',*,*,#5252,.T.);
#6961=ORIENTED_EDGE('',*,*,#5253,.T.);
#6962=ORIENTED_EDGE('',*,*,#5254,.T.);
#6963=ORIENTED_EDGE('',*,*,#5250,.F.);
#6964=ORIENTED_EDGE('',*,*,#5255,.T.);
#6965=ORIENTED_EDGE('',*,*,#5256,.T.);
#6966=ORIENTED_EDGE('',*,*,#5257,.T.);
#6967=ORIENTED_EDGE('',*,*,#5253,.F.);
#6968=ORIENTED_EDGE('',*,*,#5258,.T.);
#6969=ORIENTED_EDGE('',*,*,#5259,.T.);
#6970=ORIENTED_EDGE('',*,*,#5260,.T.);
#6971=ORIENTED_EDGE('',*,*,#5256,.F.);
#6972=ORIENTED_EDGE('',*,*,#5261,.T.);
#6973=ORIENTED_EDGE('',*,*,#5248,.T.);
#6974=ORIENTED_EDGE('',*,*,#5262,.T.);
#6975=ORIENTED_EDGE('',*,*,#5259,.F.);
#6976=ORIENTED_EDGE('',*,*,#5261,.F.);
#6977=ORIENTED_EDGE('',*,*,#5258,.F.);
#6978=ORIENTED_EDGE('',*,*,#5255,.F.);
#6979=ORIENTED_EDGE('',*,*,#5252,.F.);
#6980=ORIENTED_EDGE('',*,*,#5249,.F.);
#6981=ORIENTED_EDGE('',*,*,#5245,.F.);
#6982=ORIENTED_EDGE('',*,*,#5262,.F.);
#6983=ORIENTED_EDGE('',*,*,#5247,.F.);
#6984=ORIENTED_EDGE('',*,*,#5251,.F.);
#6985=ORIENTED_EDGE('',*,*,#5254,.F.);
#6986=ORIENTED_EDGE('',*,*,#5257,.F.);
#6987=ORIENTED_EDGE('',*,*,#5260,.F.);
#6988=ORIENTED_EDGE('',*,*,#5263,.F.);
#6989=ORIENTED_EDGE('',*,*,#5264,.F.);
#6990=ORIENTED_EDGE('',*,*,#5265,.T.);
#6991=ORIENTED_EDGE('',*,*,#5266,.F.);
#6992=ORIENTED_EDGE('',*,*,#5265,.F.);
#6993=ORIENTED_EDGE('',*,*,#5267,.F.);
#6994=ORIENTED_EDGE('',*,*,#5268,.F.);
#6995=ORIENTED_EDGE('',*,*,#5269,.F.);
#6996=ORIENTED_EDGE('',*,*,#5270,.F.);
#6997=ORIENTED_EDGE('',*,*,#5271,.F.);
#6998=ORIENTED_EDGE('',*,*,#5272,.T.);
#6999=ORIENTED_EDGE('',*,*,#5273,.F.);
#7000=ORIENTED_EDGE('',*,*,#5274,.F.);
#7001=ORIENTED_EDGE('',*,*,#5275,.F.);
#7002=ORIENTED_EDGE('',*,*,#5276,.F.);
#7003=ORIENTED_EDGE('',*,*,#5277,.F.);
#7004=ORIENTED_EDGE('',*,*,#5278,.F.);
#7005=ORIENTED_EDGE('',*,*,#5272,.F.);
#7006=ORIENTED_EDGE('',*,*,#5268,.T.);
#7007=ORIENTED_EDGE('',*,*,#5279,.T.);
#7008=ORIENTED_EDGE('',*,*,#5277,.T.);
#7009=ORIENTED_EDGE('',*,*,#5280,.F.);
#7010=ORIENTED_EDGE('',*,*,#5267,.T.);
#7011=ORIENTED_EDGE('',*,*,#5281,.T.);
#7012=ORIENTED_EDGE('',*,*,#5278,.T.);
#7013=ORIENTED_EDGE('',*,*,#5279,.F.);
#7014=ORIENTED_EDGE('',*,*,#5264,.T.);
#7015=ORIENTED_EDGE('',*,*,#5282,.T.);
#7016=ORIENTED_EDGE('',*,*,#5273,.T.);
#7017=ORIENTED_EDGE('',*,*,#5281,.F.);
#7018=ORIENTED_EDGE('',*,*,#5283,.F.);
#7019=ORIENTED_EDGE('',*,*,#5284,.T.);
#7020=ORIENTED_EDGE('',*,*,#5285,.T.);
#7021=ORIENTED_EDGE('',*,*,#5284,.F.);
#7022=ORIENTED_EDGE('',*,*,#5263,.T.);
#7023=ORIENTED_EDGE('',*,*,#5286,.T.);
#7024=ORIENTED_EDGE('',*,*,#5274,.T.);
#7025=ORIENTED_EDGE('',*,*,#5282,.F.);
#7026=ORIENTED_EDGE('',*,*,#5269,.T.);
#7027=ORIENTED_EDGE('',*,*,#5280,.T.);
#7028=ORIENTED_EDGE('',*,*,#5276,.T.);
#7029=ORIENTED_EDGE('',*,*,#5287,.F.);
#7030=ORIENTED_EDGE('',*,*,#5270,.T.);
#7031=ORIENTED_EDGE('',*,*,#5287,.T.);
#7032=ORIENTED_EDGE('',*,*,#5275,.T.);
#7033=ORIENTED_EDGE('',*,*,#5286,.F.);
#7034=ORIENTED_EDGE('',*,*,#5271,.T.);
#7035=ORIENTED_EDGE('',*,*,#5283,.T.);
#7036=ORIENTED_EDGE('',*,*,#5266,.T.);
#7037=ORIENTED_EDGE('',*,*,#5285,.F.);
#7038=ORIENTED_EDGE('',*,*,#5288,.F.);
#7039=ORIENTED_EDGE('',*,*,#5289,.T.);
#7040=ORIENTED_EDGE('',*,*,#5290,.F.);
#7041=ORIENTED_EDGE('',*,*,#5289,.F.);
#7042=ORIENTED_EDGE('',*,*,#5288,.T.);
#7043=ORIENTED_EDGE('',*,*,#5291,.F.);
#7044=ORIENTED_EDGE('',*,*,#5292,.T.);
#7045=ORIENTED_EDGE('',*,*,#5293,.F.);
#7046=ORIENTED_EDGE('',*,*,#5294,.T.);
#7047=ORIENTED_EDGE('',*,*,#5295,.F.);
#7048=ORIENTED_EDGE('',*,*,#5294,.F.);
#7049=ORIENTED_EDGE('',*,*,#5296,.F.);
#7050=ORIENTED_EDGE('',*,*,#5297,.F.);
#7051=ORIENTED_EDGE('',*,*,#5298,.F.);
#7052=ORIENTED_EDGE('',*,*,#5297,.T.);
#7053=ORIENTED_EDGE('',*,*,#5299,.T.);
#7054=ORIENTED_EDGE('',*,*,#5300,.T.);
#7055=ORIENTED_EDGE('',*,*,#5296,.T.);
#7056=ORIENTED_EDGE('',*,*,#5293,.T.);
#7057=ORIENTED_EDGE('',*,*,#5301,.T.);
#7058=ORIENTED_EDGE('',*,*,#5299,.F.);
#7059=ORIENTED_EDGE('',*,*,#5302,.F.);
#7060=ORIENTED_EDGE('',*,*,#5300,.F.);
#7061=ORIENTED_EDGE('',*,*,#5301,.F.);
#7062=ORIENTED_EDGE('',*,*,#5292,.F.);
#7063=ORIENTED_EDGE('',*,*,#5303,.T.);
#7064=ORIENTED_EDGE('',*,*,#5304,.F.);
#7065=ORIENTED_EDGE('',*,*,#5305,.F.);
#7066=ORIENTED_EDGE('',*,*,#5306,.F.);
#7067=ORIENTED_EDGE('',*,*,#5303,.F.);
#7068=ORIENTED_EDGE('',*,*,#5307,.T.);
#7069=ORIENTED_EDGE('',*,*,#5305,.T.);
#7070=ORIENTED_EDGE('',*,*,#5307,.F.);
#7071=ORIENTED_EDGE('',*,*,#5306,.T.);
#7072=ORIENTED_EDGE('',*,*,#5308,.T.);
#7073=ORIENTED_EDGE('',*,*,#5309,.T.);
#7074=ORIENTED_EDGE('',*,*,#5308,.F.);
#7075=ORIENTED_EDGE('',*,*,#5310,.F.);
#7076=ORIENTED_EDGE('',*,*,#5311,.T.);
#7077=ORIENTED_EDGE('',*,*,#5304,.T.);
#7078=ORIENTED_EDGE('',*,*,#5311,.F.);
#7079=ORIENTED_EDGE('',*,*,#5298,.T.);
#7080=ORIENTED_EDGE('',*,*,#5302,.T.);
#7081=ORIENTED_EDGE('',*,*,#5291,.T.);
#7082=ORIENTED_EDGE('',*,*,#5295,.T.);
#7083=ORIENTED_EDGE('',*,*,#5310,.T.);
#7084=ORIENTED_EDGE('',*,*,#5290,.T.);
#7085=ORIENTED_EDGE('',*,*,#5309,.F.);
#7086=ORIENTED_EDGE('',*,*,#5312,.F.);
#7087=ORIENTED_EDGE('',*,*,#5313,.T.);
#7088=ORIENTED_EDGE('',*,*,#5314,.T.);
#7089=ORIENTED_EDGE('',*,*,#5313,.F.);
#7090=ORIENTED_EDGE('',*,*,#5315,.F.);
#7091=ORIENTED_EDGE('',*,*,#5316,.T.);
#7092=ORIENTED_EDGE('',*,*,#5317,.T.);
#7093=ORIENTED_EDGE('',*,*,#5316,.F.);
#7094=ORIENTED_EDGE('',*,*,#5315,.T.);
#7095=ORIENTED_EDGE('',*,*,#5312,.T.);
#7096=ORIENTED_EDGE('',*,*,#5317,.F.);
#7097=ORIENTED_EDGE('',*,*,#5314,.F.);
#7098=ORIENTED_EDGE('',*,*,#5318,.F.);
#7099=ORIENTED_EDGE('',*,*,#5319,.T.);
#7100=ORIENTED_EDGE('',*,*,#5320,.F.);
#7101=ORIENTED_EDGE('',*,*,#5321,.F.);
#7102=ORIENTED_EDGE('',*,*,#5322,.T.);
#7103=ORIENTED_EDGE('',*,*,#5323,.F.);
#7104=ORIENTED_EDGE('',*,*,#5324,.F.);
#7105=ORIENTED_EDGE('',*,*,#5322,.F.);
#7106=ORIENTED_EDGE('',*,*,#5325,.F.);
#7107=ORIENTED_EDGE('',*,*,#5326,.F.);
#7108=ORIENTED_EDGE('',*,*,#5319,.F.);
#7109=ORIENTED_EDGE('',*,*,#5327,.F.);
#7110=ORIENTED_EDGE('',*,*,#5325,.T.);
#7111=ORIENTED_EDGE('',*,*,#5321,.T.);
#7112=ORIENTED_EDGE('',*,*,#5328,.F.);
#7113=ORIENTED_EDGE('',*,*,#5329,.T.);
#7114=ORIENTED_EDGE('',*,*,#5330,.T.);
#7115=ORIENTED_EDGE('',*,*,#5329,.F.);
#7116=ORIENTED_EDGE('',*,*,#5326,.T.);
#7117=ORIENTED_EDGE('',*,*,#5327,.T.);
#7118=ORIENTED_EDGE('',*,*,#5320,.T.);
#7119=ORIENTED_EDGE('',*,*,#5318,.T.);
#7120=ORIENTED_EDGE('',*,*,#5331,.F.);
#7121=ORIENTED_EDGE('',*,*,#5332,.T.);
#7122=ORIENTED_EDGE('',*,*,#5333,.T.);
#7123=ORIENTED_EDGE('',*,*,#5332,.F.);
#7124=ORIENTED_EDGE('',*,*,#5323,.T.);
#7125=ORIENTED_EDGE('',*,*,#5324,.T.);
#7126=ORIENTED_EDGE('',*,*,#5331,.T.);
#7127=ORIENTED_EDGE('',*,*,#5328,.T.);
#7128=ORIENTED_EDGE('',*,*,#5333,.F.);
#7129=ORIENTED_EDGE('',*,*,#5330,.F.);
#7130=ORIENTED_EDGE('',*,*,#5334,.F.);
#7131=ORIENTED_EDGE('',*,*,#5335,.T.);
#7132=ORIENTED_EDGE('',*,*,#5336,.F.);
#7133=ORIENTED_EDGE('',*,*,#5337,.F.);
#7134=ORIENTED_EDGE('',*,*,#5338,.F.);
#7135=ORIENTED_EDGE('',*,*,#5339,.T.);
#7136=ORIENTED_EDGE('',*,*,#5340,.F.);
#7137=ORIENTED_EDGE('',*,*,#5335,.F.);
#7138=ORIENTED_EDGE('',*,*,#5341,.F.);
#7139=ORIENTED_EDGE('',*,*,#5342,.F.);
#7140=ORIENTED_EDGE('',*,*,#5343,.F.);
#7141=ORIENTED_EDGE('',*,*,#5339,.F.);
#7142=ORIENTED_EDGE('',*,*,#5344,.T.);
#7143=ORIENTED_EDGE('',*,*,#5336,.T.);
#7144=ORIENTED_EDGE('',*,*,#5340,.T.);
#7145=ORIENTED_EDGE('',*,*,#5343,.T.);
#7146=ORIENTED_EDGE('',*,*,#5345,.T.);
#7147=ORIENTED_EDGE('',*,*,#5337,.T.);
#7148=ORIENTED_EDGE('',*,*,#5345,.F.);
#7149=ORIENTED_EDGE('',*,*,#5342,.T.);
#7150=ORIENTED_EDGE('',*,*,#5346,.T.);
#7151=ORIENTED_EDGE('',*,*,#5347,.F.);
#7152=ORIENTED_EDGE('',*,*,#5348,.F.);
#7153=ORIENTED_EDGE('',*,*,#5344,.F.);
#7154=ORIENTED_EDGE('',*,*,#5349,.T.);
#7155=ORIENTED_EDGE('',*,*,#5347,.T.);
#7156=ORIENTED_EDGE('',*,*,#5349,.F.);
#7157=ORIENTED_EDGE('',*,*,#5348,.T.);
#7158=ORIENTED_EDGE('',*,*,#5350,.T.);
#7159=ORIENTED_EDGE('',*,*,#5351,.T.);
#7160=ORIENTED_EDGE('',*,*,#5350,.F.);
#7161=ORIENTED_EDGE('',*,*,#5351,.F.);
#7162=ORIENTED_EDGE('',*,*,#5334,.T.);
#7163=ORIENTED_EDGE('',*,*,#5346,.F.);
#7164=ORIENTED_EDGE('',*,*,#5341,.T.);
#7165=ORIENTED_EDGE('',*,*,#5338,.T.);
#7166=ORIENTED_EDGE('',*,*,#5352,.F.);
#7167=ORIENTED_EDGE('',*,*,#5353,.T.);
#7168=ORIENTED_EDGE('',*,*,#5354,.T.);
#7169=ORIENTED_EDGE('',*,*,#5353,.F.);
#7170=ORIENTED_EDGE('',*,*,#5355,.F.);
#7171=ORIENTED_EDGE('',*,*,#5356,.T.);
#7172=ORIENTED_EDGE('',*,*,#5357,.T.);
#7173=ORIENTED_EDGE('',*,*,#5356,.F.);
#7174=ORIENTED_EDGE('',*,*,#5355,.T.);
#7175=ORIENTED_EDGE('',*,*,#5352,.T.);
#7176=ORIENTED_EDGE('',*,*,#5357,.F.);
#7177=ORIENTED_EDGE('',*,*,#5354,.F.);
#7178=ORIENTED_EDGE('',*,*,#5358,.F.);
#7179=ORIENTED_EDGE('',*,*,#5359,.T.);
#7180=ORIENTED_EDGE('',*,*,#5360,.T.);
#7181=ORIENTED_EDGE('',*,*,#5359,.F.);
#7182=ORIENTED_EDGE('',*,*,#5361,.F.);
#7183=ORIENTED_EDGE('',*,*,#5362,.T.);
#7184=ORIENTED_EDGE('',*,*,#5363,.T.);
#7185=ORIENTED_EDGE('',*,*,#5362,.F.);
#7186=ORIENTED_EDGE('',*,*,#5361,.T.);
#7187=ORIENTED_EDGE('',*,*,#5358,.T.);
#7188=ORIENTED_EDGE('',*,*,#5363,.F.);
#7189=ORIENTED_EDGE('',*,*,#5360,.F.);
#7190=ORIENTED_EDGE('',*,*,#5364,.F.);
#7191=ORIENTED_EDGE('',*,*,#5365,.F.);
#7192=ORIENTED_EDGE('',*,*,#5366,.T.);
#7193=ORIENTED_EDGE('',*,*,#5364,.T.);
#7194=ORIENTED_EDGE('',*,*,#5366,.F.);
#7195=ORIENTED_EDGE('',*,*,#5367,.F.);
#7196=ORIENTED_EDGE('',*,*,#5368,.T.);
#7197=ORIENTED_EDGE('',*,*,#5365,.T.);
#7198=ORIENTED_EDGE('',*,*,#5368,.F.);
#7199=ORIENTED_EDGE('',*,*,#5369,.F.);
#7200=ORIENTED_EDGE('',*,*,#5370,.T.);
#7201=ORIENTED_EDGE('',*,*,#5367,.T.);
#7202=ORIENTED_EDGE('',*,*,#5370,.F.);
#7203=ORIENTED_EDGE('',*,*,#5369,.T.);
#7204=ORIENTED_EDGE('',*,*,#5371,.F.);
#7205=ORIENTED_EDGE('',*,*,#5372,.F.);
#7206=ORIENTED_EDGE('',*,*,#5373,.T.);
#7207=ORIENTED_EDGE('',*,*,#5371,.T.);
#7208=ORIENTED_EDGE('',*,*,#5373,.F.);
#7209=ORIENTED_EDGE('',*,*,#5374,.F.);
#7210=ORIENTED_EDGE('',*,*,#5375,.T.);
#7211=ORIENTED_EDGE('',*,*,#5372,.T.);
#7212=ORIENTED_EDGE('',*,*,#5375,.F.);
#7213=ORIENTED_EDGE('',*,*,#5376,.F.);
#7214=ORIENTED_EDGE('',*,*,#5377,.T.);
#7215=ORIENTED_EDGE('',*,*,#5374,.T.);
#7216=ORIENTED_EDGE('',*,*,#5377,.F.);
#7217=ORIENTED_EDGE('',*,*,#5376,.T.);
#7218=ORIENTED_EDGE('',*,*,#5378,.T.);
#7219=ORIENTED_EDGE('',*,*,#5379,.T.);
#7220=ORIENTED_EDGE('',*,*,#5380,.T.);
#7221=ORIENTED_EDGE('',*,*,#5381,.F.);
#7222=ORIENTED_EDGE('',*,*,#5382,.T.);
#7223=ORIENTED_EDGE('',*,*,#5383,.T.);
#7224=ORIENTED_EDGE('',*,*,#5384,.T.);
#7225=ORIENTED_EDGE('',*,*,#5379,.F.);
#7226=ORIENTED_EDGE('',*,*,#5385,.T.);
#7227=ORIENTED_EDGE('',*,*,#5386,.T.);
#7228=ORIENTED_EDGE('',*,*,#5387,.T.);
#7229=ORIENTED_EDGE('',*,*,#5383,.F.);
#7230=ORIENTED_EDGE('',*,*,#5388,.T.);
#7231=ORIENTED_EDGE('',*,*,#5389,.T.);
#7232=ORIENTED_EDGE('',*,*,#5390,.T.);
#7233=ORIENTED_EDGE('',*,*,#5386,.F.);
#7234=ORIENTED_EDGE('',*,*,#5391,.T.);
#7235=ORIENTED_EDGE('',*,*,#5392,.T.);
#7236=ORIENTED_EDGE('',*,*,#5393,.T.);
#7237=ORIENTED_EDGE('',*,*,#5389,.F.);
#7238=ORIENTED_EDGE('',*,*,#5394,.T.);
#7239=ORIENTED_EDGE('',*,*,#5381,.T.);
#7240=ORIENTED_EDGE('',*,*,#5395,.T.);
#7241=ORIENTED_EDGE('',*,*,#5392,.F.);
#7242=ORIENTED_EDGE('',*,*,#5394,.F.);
#7243=ORIENTED_EDGE('',*,*,#5391,.F.);
#7244=ORIENTED_EDGE('',*,*,#5388,.F.);
#7245=ORIENTED_EDGE('',*,*,#5385,.F.);
#7246=ORIENTED_EDGE('',*,*,#5382,.F.);
#7247=ORIENTED_EDGE('',*,*,#5378,.F.);
#7248=ORIENTED_EDGE('',*,*,#5395,.F.);
#7249=ORIENTED_EDGE('',*,*,#5380,.F.);
#7250=ORIENTED_EDGE('',*,*,#5384,.F.);
#7251=ORIENTED_EDGE('',*,*,#5387,.F.);
#7252=ORIENTED_EDGE('',*,*,#5390,.F.);
#7253=ORIENTED_EDGE('',*,*,#5393,.F.);
#7254=ORIENTED_EDGE('',*,*,#5396,.F.);
#7255=ORIENTED_EDGE('',*,*,#5397,.T.);
#7256=ORIENTED_EDGE('',*,*,#5398,.F.);
#7257=ORIENTED_EDGE('',*,*,#5399,.F.);
#7258=ORIENTED_EDGE('',*,*,#5400,.F.);
#7259=ORIENTED_EDGE('',*,*,#5399,.T.);
#7260=ORIENTED_EDGE('',*,*,#5401,.T.);
#7261=ORIENTED_EDGE('',*,*,#5402,.T.);
#7262=ORIENTED_EDGE('',*,*,#5401,.F.);
#7263=ORIENTED_EDGE('',*,*,#5398,.T.);
#7264=ORIENTED_EDGE('',*,*,#5403,.T.);
#7265=ORIENTED_EDGE('',*,*,#5404,.F.);
#7266=ORIENTED_EDGE('',*,*,#5405,.F.);
#7267=ORIENTED_EDGE('',*,*,#5402,.F.);
#7268=ORIENTED_EDGE('',*,*,#5404,.T.);
#7269=ORIENTED_EDGE('',*,*,#5406,.T.);
#7270=ORIENTED_EDGE('',*,*,#5407,.F.);
#7271=ORIENTED_EDGE('',*,*,#5406,.F.);
#7272=ORIENTED_EDGE('',*,*,#5403,.F.);
#7273=ORIENTED_EDGE('',*,*,#5397,.F.);
#7274=ORIENTED_EDGE('',*,*,#5408,.T.);
#7275=ORIENTED_EDGE('',*,*,#5409,.F.);
#7276=ORIENTED_EDGE('',*,*,#5410,.F.);
#7277=ORIENTED_EDGE('',*,*,#5411,.F.);
#7278=ORIENTED_EDGE('',*,*,#5408,.F.);
#7279=ORIENTED_EDGE('',*,*,#5412,.T.);
#7280=ORIENTED_EDGE('',*,*,#5410,.T.);
#7281=ORIENTED_EDGE('',*,*,#5412,.F.);
#7282=ORIENTED_EDGE('',*,*,#5411,.T.);
#7283=ORIENTED_EDGE('',*,*,#5413,.T.);
#7284=ORIENTED_EDGE('',*,*,#5414,.T.);
#7285=ORIENTED_EDGE('',*,*,#5413,.F.);
#7286=ORIENTED_EDGE('',*,*,#5415,.F.);
#7287=ORIENTED_EDGE('',*,*,#5416,.T.);
#7288=ORIENTED_EDGE('',*,*,#5409,.T.);
#7289=ORIENTED_EDGE('',*,*,#5416,.F.);
#7290=ORIENTED_EDGE('',*,*,#5405,.T.);
#7291=ORIENTED_EDGE('',*,*,#5407,.T.);
#7292=ORIENTED_EDGE('',*,*,#5396,.T.);
#7293=ORIENTED_EDGE('',*,*,#5400,.T.);
#7294=ORIENTED_EDGE('',*,*,#5415,.T.);
#7295=ORIENTED_EDGE('',*,*,#5414,.F.);
#7296=ORIENTED_EDGE('',*,*,#5417,.F.);
#7297=ORIENTED_EDGE('',*,*,#5418,.T.);
#7298=ORIENTED_EDGE('',*,*,#5419,.F.);
#7299=ORIENTED_EDGE('',*,*,#5420,.F.);
#7300=ORIENTED_EDGE('',*,*,#5421,.F.);
#7301=ORIENTED_EDGE('',*,*,#5422,.T.);
#7302=ORIENTED_EDGE('',*,*,#5423,.F.);
#7303=ORIENTED_EDGE('',*,*,#5418,.F.);
#7304=ORIENTED_EDGE('',*,*,#5424,.F.);
#7305=ORIENTED_EDGE('',*,*,#5425,.F.);
#7306=ORIENTED_EDGE('',*,*,#5426,.F.);
#7307=ORIENTED_EDGE('',*,*,#5422,.F.);
#7308=ORIENTED_EDGE('',*,*,#5427,.T.);
#7309=ORIENTED_EDGE('',*,*,#5419,.T.);
#7310=ORIENTED_EDGE('',*,*,#5423,.T.);
#7311=ORIENTED_EDGE('',*,*,#5426,.T.);
#7312=ORIENTED_EDGE('',*,*,#5428,.T.);
#7313=ORIENTED_EDGE('',*,*,#5420,.T.);
#7314=ORIENTED_EDGE('',*,*,#5428,.F.);
#7315=ORIENTED_EDGE('',*,*,#5425,.T.);
#7316=ORIENTED_EDGE('',*,*,#5429,.T.);
#7317=ORIENTED_EDGE('',*,*,#5430,.T.);
#7318=ORIENTED_EDGE('',*,*,#5431,.F.);
#7319=ORIENTED_EDGE('',*,*,#5430,.F.);
#7320=ORIENTED_EDGE('',*,*,#5432,.T.);
#7321=ORIENTED_EDGE('',*,*,#5433,.T.);
#7322=ORIENTED_EDGE('',*,*,#5432,.F.);
#7323=ORIENTED_EDGE('',*,*,#5427,.F.);
#7324=ORIENTED_EDGE('',*,*,#5434,.T.);
#7325=ORIENTED_EDGE('',*,*,#5431,.T.);
#7326=ORIENTED_EDGE('',*,*,#5434,.F.);
#7327=ORIENTED_EDGE('',*,*,#5433,.F.);
#7328=ORIENTED_EDGE('',*,*,#5417,.T.);
#7329=ORIENTED_EDGE('',*,*,#5429,.F.);
#7330=ORIENTED_EDGE('',*,*,#5424,.T.);
#7331=ORIENTED_EDGE('',*,*,#5421,.T.);
#7332=ORIENTED_EDGE('',*,*,#5435,.F.);
#7333=ORIENTED_EDGE('',*,*,#5436,.T.);
#7334=ORIENTED_EDGE('',*,*,#5437,.T.);
#7335=ORIENTED_EDGE('',*,*,#5436,.F.);
#7336=ORIENTED_EDGE('',*,*,#5438,.F.);
#7337=ORIENTED_EDGE('',*,*,#5439,.T.);
#7338=ORIENTED_EDGE('',*,*,#5440,.T.);
#7339=ORIENTED_EDGE('',*,*,#5439,.F.);
#7340=ORIENTED_EDGE('',*,*,#5438,.T.);
#7341=ORIENTED_EDGE('',*,*,#5435,.T.);
#7342=ORIENTED_EDGE('',*,*,#5440,.F.);
#7343=ORIENTED_EDGE('',*,*,#5437,.F.);
#7344=ORIENTED_EDGE('',*,*,#5441,.F.);
#7345=ORIENTED_EDGE('',*,*,#5442,.T.);
#7346=ORIENTED_EDGE('',*,*,#5443,.T.);
#7347=ORIENTED_EDGE('',*,*,#5442,.F.);
#7348=ORIENTED_EDGE('',*,*,#5444,.F.);
#7349=ORIENTED_EDGE('',*,*,#5445,.T.);
#7350=ORIENTED_EDGE('',*,*,#5446,.T.);
#7351=ORIENTED_EDGE('',*,*,#5445,.F.);
#7352=ORIENTED_EDGE('',*,*,#5444,.T.);
#7353=ORIENTED_EDGE('',*,*,#5441,.T.);
#7354=ORIENTED_EDGE('',*,*,#5446,.F.);
#7355=ORIENTED_EDGE('',*,*,#5443,.F.);
#7356=ORIENTED_EDGE('',*,*,#5447,.F.);
#7357=ORIENTED_EDGE('',*,*,#5448,.T.);
#7358=ORIENTED_EDGE('',*,*,#5449,.F.);
#7359=ORIENTED_EDGE('',*,*,#5450,.F.);
#7360=ORIENTED_EDGE('',*,*,#5451,.F.);
#7361=ORIENTED_EDGE('',*,*,#5452,.F.);
#7362=ORIENTED_EDGE('',*,*,#5448,.F.);
#7363=ORIENTED_EDGE('',*,*,#5453,.F.);
#7364=ORIENTED_EDGE('',*,*,#5454,.T.);
#7365=ORIENTED_EDGE('',*,*,#5455,.F.);
#7366=ORIENTED_EDGE('',*,*,#5456,.F.);
#7367=ORIENTED_EDGE('',*,*,#5457,.F.);
#7368=ORIENTED_EDGE('',*,*,#5454,.F.);
#7369=ORIENTED_EDGE('',*,*,#5458,.F.);
#7370=ORIENTED_EDGE('',*,*,#5450,.T.);
#7371=ORIENTED_EDGE('',*,*,#5459,.F.);
#7372=ORIENTED_EDGE('',*,*,#5460,.T.);
#7373=ORIENTED_EDGE('',*,*,#5451,.T.);
#7374=ORIENTED_EDGE('',*,*,#5458,.T.);
#7375=ORIENTED_EDGE('',*,*,#5449,.T.);
#7376=ORIENTED_EDGE('',*,*,#5461,.T.);
#7377=ORIENTED_EDGE('',*,*,#5462,.T.);
#7378=ORIENTED_EDGE('',*,*,#5461,.F.);
#7379=ORIENTED_EDGE('',*,*,#5453,.T.);
#7380=ORIENTED_EDGE('',*,*,#5447,.T.);
#7381=ORIENTED_EDGE('',*,*,#5452,.T.);
#7382=ORIENTED_EDGE('',*,*,#5460,.F.);
#7383=ORIENTED_EDGE('',*,*,#5463,.F.);
#7384=ORIENTED_EDGE('',*,*,#5464,.T.);
#7385=ORIENTED_EDGE('',*,*,#5456,.T.);
#7386=ORIENTED_EDGE('',*,*,#5455,.T.);
#7387=ORIENTED_EDGE('',*,*,#5465,.T.);
#7388=ORIENTED_EDGE('',*,*,#5466,.T.);
#7389=ORIENTED_EDGE('',*,*,#5465,.F.);
#7390=ORIENTED_EDGE('',*,*,#5457,.T.);
#7391=ORIENTED_EDGE('',*,*,#5464,.F.);
#7392=ORIENTED_EDGE('',*,*,#5463,.T.);
#7393=ORIENTED_EDGE('',*,*,#5459,.T.);
#7394=ORIENTED_EDGE('',*,*,#5466,.F.);
#7395=ORIENTED_EDGE('',*,*,#5462,.F.);
#7396=ORIENTED_EDGE('',*,*,#5467,.F.);
#7397=ORIENTED_EDGE('',*,*,#5468,.T.);
#7398=ORIENTED_EDGE('',*,*,#5469,.F.);
#7399=ORIENTED_EDGE('',*,*,#5470,.F.);
#7400=ORIENTED_EDGE('',*,*,#5471,.F.);
#7401=ORIENTED_EDGE('',*,*,#5472,.F.);
#7402=ORIENTED_EDGE('',*,*,#5468,.F.);
#7403=ORIENTED_EDGE('',*,*,#5473,.F.);
#7404=ORIENTED_EDGE('',*,*,#5474,.T.);
#7405=ORIENTED_EDGE('',*,*,#5475,.F.);
#7406=ORIENTED_EDGE('',*,*,#5476,.F.);
#7407=ORIENTED_EDGE('',*,*,#5477,.F.);
#7408=ORIENTED_EDGE('',*,*,#5474,.F.);
#7409=ORIENTED_EDGE('',*,*,#5478,.F.);
#7410=ORIENTED_EDGE('',*,*,#5470,.T.);
#7411=ORIENTED_EDGE('',*,*,#5479,.F.);
#7412=ORIENTED_EDGE('',*,*,#5480,.T.);
#7413=ORIENTED_EDGE('',*,*,#5471,.T.);
#7414=ORIENTED_EDGE('',*,*,#5478,.T.);
#7415=ORIENTED_EDGE('',*,*,#5469,.T.);
#7416=ORIENTED_EDGE('',*,*,#5481,.T.);
#7417=ORIENTED_EDGE('',*,*,#5482,.T.);
#7418=ORIENTED_EDGE('',*,*,#5481,.F.);
#7419=ORIENTED_EDGE('',*,*,#5473,.T.);
#7420=ORIENTED_EDGE('',*,*,#5467,.T.);
#7421=ORIENTED_EDGE('',*,*,#5472,.T.);
#7422=ORIENTED_EDGE('',*,*,#5480,.F.);
#7423=ORIENTED_EDGE('',*,*,#5483,.F.);
#7424=ORIENTED_EDGE('',*,*,#5484,.T.);
#7425=ORIENTED_EDGE('',*,*,#5476,.T.);
#7426=ORIENTED_EDGE('',*,*,#5475,.T.);
#7427=ORIENTED_EDGE('',*,*,#5485,.T.);
#7428=ORIENTED_EDGE('',*,*,#5486,.T.);
#7429=ORIENTED_EDGE('',*,*,#5485,.F.);
#7430=ORIENTED_EDGE('',*,*,#5477,.T.);
#7431=ORIENTED_EDGE('',*,*,#5484,.F.);
#7432=ORIENTED_EDGE('',*,*,#5483,.T.);
#7433=ORIENTED_EDGE('',*,*,#5479,.T.);
#7434=ORIENTED_EDGE('',*,*,#5486,.F.);
#7435=ORIENTED_EDGE('',*,*,#5482,.F.);
#7436=ORIENTED_EDGE('',*,*,#5487,.F.);
#7437=ORIENTED_EDGE('',*,*,#5488,.F.);
#7438=ORIENTED_EDGE('',*,*,#5489,.F.);
#7439=ORIENTED_EDGE('',*,*,#5490,.F.);
#7440=ORIENTED_EDGE('',*,*,#5491,.F.);
#7441=ORIENTED_EDGE('',*,*,#5492,.F.);
#7442=ORIENTED_EDGE('',*,*,#5493,.F.);
#7443=ORIENTED_EDGE('',*,*,#5494,.F.);
#7444=ORIENTED_EDGE('',*,*,#5491,.T.);
#7445=ORIENTED_EDGE('',*,*,#5495,.T.);
#7446=ORIENTED_EDGE('',*,*,#5496,.T.);
#7447=ORIENTED_EDGE('',*,*,#5497,.T.);
#7448=ORIENTED_EDGE('',*,*,#5490,.T.);
#7449=ORIENTED_EDGE('',*,*,#5498,.F.);
#7450=ORIENTED_EDGE('',*,*,#5499,.T.);
#7451=ORIENTED_EDGE('',*,*,#5495,.F.);
#7452=ORIENTED_EDGE('',*,*,#5489,.T.);
#7453=ORIENTED_EDGE('',*,*,#5500,.T.);
#7454=ORIENTED_EDGE('',*,*,#5501,.T.);
#7455=ORIENTED_EDGE('',*,*,#5498,.T.);
#7456=ORIENTED_EDGE('',*,*,#5488,.T.);
#7457=ORIENTED_EDGE('',*,*,#5502,.F.);
#7458=ORIENTED_EDGE('',*,*,#5503,.T.);
#7459=ORIENTED_EDGE('',*,*,#5500,.F.);
#7460=ORIENTED_EDGE('',*,*,#5496,.F.);
#7461=ORIENTED_EDGE('',*,*,#5499,.F.);
#7462=ORIENTED_EDGE('',*,*,#5501,.F.);
#7463=ORIENTED_EDGE('',*,*,#5503,.F.);
#7464=ORIENTED_EDGE('',*,*,#5504,.F.);
#7465=ORIENTED_EDGE('',*,*,#5505,.F.);
#7466=ORIENTED_EDGE('',*,*,#5506,.F.);
#7467=ORIENTED_EDGE('',*,*,#5507,.F.);
#7468=ORIENTED_EDGE('',*,*,#5487,.T.);
#7469=ORIENTED_EDGE('',*,*,#5508,.T.);
#7470=ORIENTED_EDGE('',*,*,#5504,.T.);
#7471=ORIENTED_EDGE('',*,*,#5502,.T.);
#7472=ORIENTED_EDGE('',*,*,#5494,.T.);
#7473=ORIENTED_EDGE('',*,*,#5509,.F.);
#7474=ORIENTED_EDGE('',*,*,#5505,.T.);
#7475=ORIENTED_EDGE('',*,*,#5508,.F.);
#7476=ORIENTED_EDGE('',*,*,#5493,.T.);
#7477=ORIENTED_EDGE('',*,*,#5510,.T.);
#7478=ORIENTED_EDGE('',*,*,#5506,.T.);
#7479=ORIENTED_EDGE('',*,*,#5509,.T.);
#7480=ORIENTED_EDGE('',*,*,#5492,.T.);
#7481=ORIENTED_EDGE('',*,*,#5497,.F.);
#7482=ORIENTED_EDGE('',*,*,#5507,.T.);
#7483=ORIENTED_EDGE('',*,*,#5510,.F.);
#7484=ORIENTED_EDGE('',*,*,#5511,.F.);
#7485=ORIENTED_EDGE('',*,*,#5512,.F.);
#7486=ORIENTED_EDGE('',*,*,#5513,.T.);
#7487=ORIENTED_EDGE('',*,*,#5514,.T.);
#7488=ORIENTED_EDGE('',*,*,#5515,.F.);
#7489=ORIENTED_EDGE('',*,*,#5516,.F.);
#7490=ORIENTED_EDGE('',*,*,#5517,.T.);
#7491=ORIENTED_EDGE('',*,*,#5518,.T.);
#7492=ORIENTED_EDGE('',*,*,#5513,.F.);
#7493=ORIENTED_EDGE('',*,*,#5519,.F.);
#7494=ORIENTED_EDGE('',*,*,#5520,.T.);
#7495=ORIENTED_EDGE('',*,*,#5521,.T.);
#7496=ORIENTED_EDGE('',*,*,#5517,.F.);
#7497=ORIENTED_EDGE('',*,*,#5522,.F.);
#7498=ORIENTED_EDGE('',*,*,#5523,.T.);
#7499=ORIENTED_EDGE('',*,*,#5524,.T.);
#7500=ORIENTED_EDGE('',*,*,#5520,.F.);
#7501=ORIENTED_EDGE('',*,*,#5525,.F.);
#7502=ORIENTED_EDGE('',*,*,#5526,.T.);
#7503=ORIENTED_EDGE('',*,*,#5527,.T.);
#7504=ORIENTED_EDGE('',*,*,#5523,.F.);
#7505=ORIENTED_EDGE('',*,*,#5528,.F.);
#7506=ORIENTED_EDGE('',*,*,#5515,.T.);
#7507=ORIENTED_EDGE('',*,*,#5529,.T.);
#7508=ORIENTED_EDGE('',*,*,#5526,.F.);
#7509=ORIENTED_EDGE('',*,*,#5529,.F.);
#7510=ORIENTED_EDGE('',*,*,#5514,.F.);
#7511=ORIENTED_EDGE('',*,*,#5518,.F.);
#7512=ORIENTED_EDGE('',*,*,#5521,.F.);
#7513=ORIENTED_EDGE('',*,*,#5524,.F.);
#7514=ORIENTED_EDGE('',*,*,#5527,.F.);
#7515=ORIENTED_EDGE('',*,*,#5530,.F.);
#7516=ORIENTED_EDGE('',*,*,#5512,.T.);
#7517=ORIENTED_EDGE('',*,*,#5528,.T.);
#7518=ORIENTED_EDGE('',*,*,#5525,.T.);
#7519=ORIENTED_EDGE('',*,*,#5522,.T.);
#7520=ORIENTED_EDGE('',*,*,#5519,.T.);
#7521=ORIENTED_EDGE('',*,*,#5516,.T.);
#7522=ORIENTED_EDGE('',*,*,#5531,.F.);
#7523=ORIENTED_EDGE('',*,*,#5532,.T.);
#7524=ORIENTED_EDGE('',*,*,#5530,.T.);
#7525=ORIENTED_EDGE('',*,*,#5532,.F.);
#7526=ORIENTED_EDGE('',*,*,#5511,.T.);
#7527=ORIENTED_EDGE('',*,*,#5533,.T.);
#7528=ORIENTED_EDGE('',*,*,#5531,.T.);
#7529=ORIENTED_EDGE('',*,*,#5533,.F.);
#7530=CYLINDRICAL_SURFACE('',#8745,0.165);
#7531=CYLINDRICAL_SURFACE('',#8748,0.165);
#7532=CYLINDRICAL_SURFACE('',#8751,0.165);
#7533=CYLINDRICAL_SURFACE('',#8754,0.165);
#7534=CYLINDRICAL_SURFACE('',#8757,0.165);
#7535=CYLINDRICAL_SURFACE('',#8760,0.165);
#7536=CYLINDRICAL_SURFACE('',#8763,0.210000000000001);
#7537=CYLINDRICAL_SURFACE('',#8766,0.21);
#7538=CYLINDRICAL_SURFACE('',#8769,0.21);
#7539=CYLINDRICAL_SURFACE('',#8772,0.210000000000001);
#7540=CYLINDRICAL_SURFACE('',#8796,0.165);
#7541=CYLINDRICAL_SURFACE('',#8799,0.165);
#7542=CYLINDRICAL_SURFACE('',#8802,0.165);
#7543=CYLINDRICAL_SURFACE('',#8805,0.165);
#7544=CYLINDRICAL_SURFACE('',#8808,0.275);
#7545=CYLINDRICAL_SURFACE('',#8811,0.275);
#7546=CYLINDRICAL_SURFACE('',#8823,0.275);
#7547=CYLINDRICAL_SURFACE('',#8825,0.275);
#7548=CYLINDRICAL_SURFACE('',#8829,0.275);
#7549=CYLINDRICAL_SURFACE('',#8831,0.275);
#7550=CYLINDRICAL_SURFACE('',#8835,0.275);
#7551=CYLINDRICAL_SURFACE('',#8837,0.275);
#7552=CYLINDRICAL_SURFACE('',#8847,0.165);
#7553=CYLINDRICAL_SURFACE('',#8850,0.165);
#7554=CYLINDRICAL_SURFACE('',#8853,0.165);
#7555=CYLINDRICAL_SURFACE('',#8856,0.165);
#7556=CYLINDRICAL_SURFACE('',#8859,1.6);
#7557=CYLINDRICAL_SURFACE('',#8862,0.225);
#7558=CYLINDRICAL_SURFACE('',#8865,0.225);
#7559=CYLINDRICAL_SURFACE('',#8879,0.225);
#7560=CYLINDRICAL_SURFACE('',#8882,0.225);
#7561=CYLINDRICAL_SURFACE('',#8885,0.225);
#7562=CYLINDRICAL_SURFACE('',#8888,0.225);
#7563=CYLINDRICAL_SURFACE('',#8891,1.59);
#7564=CYLINDRICAL_SURFACE('',#8896,1.2);
#7565=CYLINDRICAL_SURFACE('',#8898,2.4);
#7566=CYLINDRICAL_SURFACE('',#8904,0.225);
#7567=CYLINDRICAL_SURFACE('',#8907,0.225);
#7568=CYLINDRICAL_SURFACE('',#8910,0.225);
#7569=CYLINDRICAL_SURFACE('',#8913,0.225);
#7570=CYLINDRICAL_SURFACE('',#8916,1.59);
#7571=CYLINDRICAL_SURFACE('',#8921,1.2);
#7572=CYLINDRICAL_SURFACE('',#8923,2.4);
#7573=CYLINDRICAL_SURFACE('',#8929,0.165);
#7574=CYLINDRICAL_SURFACE('',#8932,0.165);
#7575=CYLINDRICAL_SURFACE('',#8935,0.165);
#7576=CYLINDRICAL_SURFACE('',#8938,0.165);
#7577=CYLINDRICAL_SURFACE('',#8941,1.6);
#7578=CYLINDRICAL_SURFACE('',#8944,0.225);
#7579=CYLINDRICAL_SURFACE('',#8947,0.225);
#7580=CYLINDRICAL_SURFACE('',#8961,0.225);
#7581=CYLINDRICAL_SURFACE('',#8964,0.225);
#7582=CYLINDRICAL_SURFACE('',#8967,0.225);
#7583=CYLINDRICAL_SURFACE('',#8970,0.225);
#7584=CYLINDRICAL_SURFACE('',#8973,1.59);
#7585=CYLINDRICAL_SURFACE('',#8978,1.2);
#7586=CYLINDRICAL_SURFACE('',#8980,2.4);
#7587=CYLINDRICAL_SURFACE('',#8986,0.225);
#7588=CYLINDRICAL_SURFACE('',#8989,0.225);
#7589=CYLINDRICAL_SURFACE('',#8992,0.225);
#7590=CYLINDRICAL_SURFACE('',#8995,0.225);
#7591=CYLINDRICAL_SURFACE('',#8998,1.59);
#7592=CYLINDRICAL_SURFACE('',#9003,1.2);
#7593=CYLINDRICAL_SURFACE('',#9005,2.4);
#7594=CYLINDRICAL_SURFACE('',#9011,0.165);
#7595=CYLINDRICAL_SURFACE('',#9014,0.164999999999999);
#7596=CYLINDRICAL_SURFACE('',#9017,0.164999999999999);
#7597=CYLINDRICAL_SURFACE('',#9020,0.165);
#7598=CYLINDRICAL_SURFACE('',#9023,1.6);
#7599=CYLINDRICAL_SURFACE('',#9026,0.225);
#7600=CYLINDRICAL_SURFACE('',#9029,0.225);
#7601=CYLINDRICAL_SURFACE('',#9043,0.225);
#7602=CYLINDRICAL_SURFACE('',#9046,0.225);
#7603=CYLINDRICAL_SURFACE('',#9049,0.225);
#7604=CYLINDRICAL_SURFACE('',#9052,0.225);
#7605=CYLINDRICAL_SURFACE('',#9055,1.59);
#7606=CYLINDRICAL_SURFACE('',#9060,1.2);
#7607=CYLINDRICAL_SURFACE('',#9062,2.4);
#7608=CYLINDRICAL_SURFACE('',#9068,0.225);
#7609=CYLINDRICAL_SURFACE('',#9071,0.225);
#7610=CYLINDRICAL_SURFACE('',#9074,0.225);
#7611=CYLINDRICAL_SURFACE('',#9077,0.225);
#7612=CYLINDRICAL_SURFACE('',#9080,1.59);
#7613=CYLINDRICAL_SURFACE('',#9085,1.2);
#7614=CYLINDRICAL_SURFACE('',#9087,2.4);
#7615=CYLINDRICAL_SURFACE('',#9093,0.165);
#7616=CYLINDRICAL_SURFACE('',#9096,0.164999999999999);
#7617=CYLINDRICAL_SURFACE('',#9099,0.164999999999999);
#7618=CYLINDRICAL_SURFACE('',#9102,0.165);
#7619=CYLINDRICAL_SURFACE('',#9105,1.6);
#7620=CYLINDRICAL_SURFACE('',#9108,0.225);
#7621=CYLINDRICAL_SURFACE('',#9111,0.225);
#7622=CYLINDRICAL_SURFACE('',#9125,0.225);
#7623=CYLINDRICAL_SURFACE('',#9128,0.225);
#7624=CYLINDRICAL_SURFACE('',#9131,0.225);
#7625=CYLINDRICAL_SURFACE('',#9134,0.225);
#7626=CYLINDRICAL_SURFACE('',#9137,1.59);
#7627=CYLINDRICAL_SURFACE('',#9142,1.2);
#7628=CYLINDRICAL_SURFACE('',#9144,2.4);
#7629=CYLINDRICAL_SURFACE('',#9150,0.225);
#7630=CYLINDRICAL_SURFACE('',#9153,0.225);
#7631=CYLINDRICAL_SURFACE('',#9156,0.225);
#7632=CYLINDRICAL_SURFACE('',#9159,0.225);
#7633=CYLINDRICAL_SURFACE('',#9162,1.59);
#7634=CYLINDRICAL_SURFACE('',#9167,1.2);
#7635=CYLINDRICAL_SURFACE('',#9169,2.4);
#7636=CYLINDRICAL_SURFACE('',#9175,0.25);
#7637=CYLINDRICAL_SURFACE('',#9178,0.25);
#7638=CYLINDRICAL_SURFACE('',#9181,0.4);
#7639=CYLINDRICAL_SURFACE('',#9186,0.225);
#7640=CYLINDRICAL_SURFACE('',#9188,0.4);
#7641=CYLINDRICAL_SURFACE('',#9193,0.225);
#7642=CYLINDRICAL_SURFACE('',#9202,0.7);
#7643=CYLINDRICAL_SURFACE('',#9208,0.7);
#7644=CYLINDRICAL_SURFACE('',#9219,0.7);
#7645=CYLINDRICAL_SURFACE('',#9225,0.7);
#7646=CYLINDRICAL_SURFACE('',#9240,0.425);
#7647=CYLINDRICAL_SURFACE('',#9248,0.24505);
#7648=CYLINDRICAL_SURFACE('',#9269,1.070235);
#7649=CYLINDRICAL_SURFACE('',#9271,0.6);
#7650=CYLINDRICAL_SURFACE('',#9277,1.070235);
#7651=CYLINDRICAL_SURFACE('',#9289,1.129765);
#7652=CYLINDRICAL_SURFACE('',#9296,1.6);
#7653=CYLINDRICAL_SURFACE('',#9301,1.129765);
#7654=CYLINDRICAL_SURFACE('',#9321,1.123812);
#7655=CYLINDRICAL_SURFACE('',#9357,1.076188);
#7656=CYLINDRICAL_SURFACE('',#9371,1.119765);
#7657=CYLINDRICAL_SURFACE('',#9375,1.085235);
#7658=CYLINDRICAL_SURFACE('',#9379,1.119765);
#7659=CYLINDRICAL_SURFACE('',#9383,1.085235);
#7660=CYLINDRICAL_SURFACE('',#9404,0.35);
#7661=CYLINDRICAL_SURFACE('',#9412,0.1954);
#7662=CYLINDRICAL_SURFACE('',#9418,0.5);
#7663=CYLINDRICAL_SURFACE('',#9426,0.2942);
#7664=CYLINDRICAL_SURFACE('',#9447,0.25175);
#7665=CYLINDRICAL_SURFACE('',#9457,0.165);
#7666=CYLINDRICAL_SURFACE('',#9474,0.8);
#7667=CYLINDRICAL_SURFACE('',#9475,0.6);
#7668=CYLINDRICAL_SURFACE('',#9477,0.6);
#7669=CYLINDRICAL_SURFACE('',#9482,0.605);
#7670=CYLINDRICAL_SURFACE('',#9485,0.8);
#7671=CYLINDRICAL_SURFACE('',#9493,0.21);
#7672=CYLINDRICAL_SURFACE('',#9497,0.605);
#7673=CYLINDRICAL_SURFACE('',#9500,1.1);
#7674=CYLINDRICAL_SURFACE('',#9512,0.6);
#7675=CYLINDRICAL_SURFACE('',#9517,3.);
#7676=CYLINDRICAL_SURFACE('',#9518,1.2);
#7677=CYLINDRICAL_SURFACE('',#9522,0.605);
#7678=CYLINDRICAL_SURFACE('',#9525,3.);
#7679=CYLINDRICAL_SURFACE('',#9531,0.225);
#7680=CYLINDRICAL_SURFACE('',#9534,0.9);
#7681=CYLINDRICAL_SURFACE('',#9544,0.35);
#7682=CYLINDRICAL_SURFACE('',#9552,0.1954);
#7683=CYLINDRICAL_SURFACE('',#9657,0.8);
#7684=CYLINDRICAL_SURFACE('',#9658,0.6);
#7685=CYLINDRICAL_SURFACE('',#9660,0.6);
#7686=CYLINDRICAL_SURFACE('',#9671,0.6);
#7687=CYLINDRICAL_SURFACE('',#9676,2.9);
#7688=CYLINDRICAL_SURFACE('',#9678,1.2);
#7689=CYLINDRICAL_SURFACE('',#9681,2.9);
#7690=CYLINDRICAL_SURFACE('',#9684,3.);
#7691=CYLINDRICAL_SURFACE('',#9690,0.605);
#7692=CYLINDRICAL_SURFACE('',#9693,0.8);
#7693=CYLINDRICAL_SURFACE('',#9701,0.21);
#7694=CYLINDRICAL_SURFACE('',#9704,0.605);
#7695=CYLINDRICAL_SURFACE('',#9707,1.1);
#7696=CYLINDRICAL_SURFACE('',#9715,0.21);
#7697=CYLINDRICAL_SURFACE('',#9718,0.605);
#7698=CYLINDRICAL_SURFACE('',#9721,1.1);
#7699=CYLINDRICAL_SURFACE('',#9751,0.24505);
#7700=ADVANCED_FACE('',(#1208),#7530,.F.);
#7701=ADVANCED_FACE('',(#1209),#7531,.F.);
#7702=ADVANCED_FACE('',(#1210),#7532,.F.);
#7703=ADVANCED_FACE('',(#1211),#7533,.F.);
#7704=ADVANCED_FACE('',(#1212),#7534,.F.);
#7705=ADVANCED_FACE('',(#1213),#7535,.F.);
#7706=ADVANCED_FACE('',(#1214),#7536,.F.);
#7707=ADVANCED_FACE('',(#1215),#7537,.F.);
#7708=ADVANCED_FACE('',(#1216),#7538,.F.);
#7709=ADVANCED_FACE('',(#1217),#7539,.F.);
#7710=ADVANCED_FACE('',(#1218),#952,.T.);
#7711=ADVANCED_FACE('',(#1219),#953,.T.);
#7712=ADVANCED_FACE('',(#1220),#954,.T.);
#7713=ADVANCED_FACE('',(#1221),#955,.T.);
#7714=ADVANCED_FACE('',(#1222,#715,#716,#717,#718,#719,#720,#721,#722,#723,
#724),#956,.T.);
#7715=ADVANCED_FACE('',(#1223,#725,#726,#727,#728,#729,#730,#731,#732,#733,
#734),#957,.F.);
#7716=ADVANCED_FACE('',(#1224),#958,.T.);
#7717=ADVANCED_FACE('',(#1225),#959,.T.);
#7718=ADVANCED_FACE('',(#1226),#960,.T.);
#7719=ADVANCED_FACE('',(#1227),#961,.T.);
#7720=ADVANCED_FACE('',(#1228),#962,.T.);
#7721=ADVANCED_FACE('',(#1229),#963,.F.);
#7722=ADVANCED_FACE('',(#1230),#964,.T.);
#7723=ADVANCED_FACE('',(#1231),#965,.T.);
#7724=ADVANCED_FACE('',(#1232),#966,.T.);
#7725=ADVANCED_FACE('',(#1233),#967,.T.);
#7726=ADVANCED_FACE('',(#1234),#968,.T.);
#7727=ADVANCED_FACE('',(#1235),#969,.F.);
#7728=ADVANCED_FACE('',(#1236),#7540,.F.);
#7729=ADVANCED_FACE('',(#1237),#7541,.F.);
#7730=ADVANCED_FACE('',(#1238),#7542,.F.);
#7731=ADVANCED_FACE('',(#1239),#7543,.F.);
#7732=ADVANCED_FACE('',(#1240),#7544,.F.);
#7733=ADVANCED_FACE('',(#1241),#7545,.F.);
#7734=ADVANCED_FACE('',(#1242,#735,#736,#737,#738,#739,#740,#741,#742),
#970,.T.);
#7735=ADVANCED_FACE('',(#1243),#971,.F.);
#7736=ADVANCED_FACE('',(#1244),#972,.F.);
#7737=ADVANCED_FACE('',(#1245),#7546,.F.);
#7738=ADVANCED_FACE('',(#1246),#7547,.F.);
#7739=ADVANCED_FACE('',(#1247),#973,.F.);
#7740=ADVANCED_FACE('',(#1248),#974,.F.);
#7741=ADVANCED_FACE('',(#1249),#7548,.F.);
#7742=ADVANCED_FACE('',(#1250),#7549,.F.);
#7743=ADVANCED_FACE('',(#1251),#975,.F.);
#7744=ADVANCED_FACE('',(#1252),#976,.F.);
#7745=ADVANCED_FACE('',(#1253),#7550,.F.);
#7746=ADVANCED_FACE('',(#1254),#7551,.F.);
#7747=ADVANCED_FACE('',(#1255),#977,.F.);
#7748=ADVANCED_FACE('',(#1256),#978,.F.);
#7749=ADVANCED_FACE('',(#1257),#979,.T.);
#7750=ADVANCED_FACE('',(#1258),#980,.T.);
#7751=ADVANCED_FACE('',(#1259),#981,.T.);
#7752=ADVANCED_FACE('',(#1260),#982,.T.);
#7753=ADVANCED_FACE('',(#1261,#743,#744,#745,#746,#747,#748,#749,#750),
#983,.F.);
#7754=ADVANCED_FACE('',(#1262),#7552,.F.);
#7755=ADVANCED_FACE('',(#1263),#7553,.F.);
#7756=ADVANCED_FACE('',(#1264),#7554,.F.);
#7757=ADVANCED_FACE('',(#1265),#7555,.F.);
#7758=ADVANCED_FACE('',(#1266),#7556,.F.);
#7759=ADVANCED_FACE('',(#1267),#7557,.F.);
#7760=ADVANCED_FACE('',(#1268),#7558,.F.);
#7761=ADVANCED_FACE('',(#1269,#751),#984,.T.);
#7762=ADVANCED_FACE('',(#1270,#752),#985,.T.);
#7763=ADVANCED_FACE('',(#1271),#986,.T.);
#7764=ADVANCED_FACE('',(#1272),#987,.T.);
#7765=ADVANCED_FACE('',(#1273,#753,#754,#755,#756,#757),#988,.T.);
#7766=ADVANCED_FACE('',(#1274),#989,.T.);
#7767=ADVANCED_FACE('',(#1275,#758,#759,#760,#761,#762),#990,.T.);
#7768=ADVANCED_FACE('',(#1276),#991,.T.);
#7769=ADVANCED_FACE('',(#1277),#992,.T.);
#7770=ADVANCED_FACE('',(#1278,#763,#764),#993,.F.);
#7771=ADVANCED_FACE('',(#1279),#7559,.F.);
#7772=ADVANCED_FACE('',(#1280),#7560,.F.);
#7773=ADVANCED_FACE('',(#1281),#7561,.F.);
#7774=ADVANCED_FACE('',(#1282),#7562,.F.);
#7775=ADVANCED_FACE('',(#1283),#7563,.T.);
#7776=ADVANCED_FACE('',(#1284,#765),#994,.T.);
#7777=ADVANCED_FACE('',(#1285),#7564,.F.);
#7778=ADVANCED_FACE('',(#1286),#7565,.T.);
#7779=ADVANCED_FACE('',(#1287,#766,#767,#768,#769,#770),#995,.T.);
#7780=ADVANCED_FACE('',(#1288,#771,#772,#773,#774,#775),#996,.F.);
#7781=ADVANCED_FACE('',(#1289),#7566,.F.);
#7782=ADVANCED_FACE('',(#1290),#7567,.F.);
#7783=ADVANCED_FACE('',(#1291),#7568,.F.);
#7784=ADVANCED_FACE('',(#1292),#7569,.F.);
#7785=ADVANCED_FACE('',(#1293),#7570,.T.);
#7786=ADVANCED_FACE('',(#1294,#776),#997,.F.);
#7787=ADVANCED_FACE('',(#1295),#7571,.F.);
#7788=ADVANCED_FACE('',(#1296),#7572,.T.);
#7789=ADVANCED_FACE('',(#1297,#777,#778,#779,#780,#781),#998,.T.);
#7790=ADVANCED_FACE('',(#1298,#782,#783,#784,#785,#786),#999,.F.);
#7791=ADVANCED_FACE('',(#1299),#7573,.F.);
#7792=ADVANCED_FACE('',(#1300),#7574,.F.);
#7793=ADVANCED_FACE('',(#1301),#7575,.F.);
#7794=ADVANCED_FACE('',(#1302),#7576,.F.);
#7795=ADVANCED_FACE('',(#1303),#7577,.F.);
#7796=ADVANCED_FACE('',(#1304),#7578,.F.);
#7797=ADVANCED_FACE('',(#1305),#7579,.F.);
#7798=ADVANCED_FACE('',(#1306,#787),#1000,.T.);
#7799=ADVANCED_FACE('',(#1307,#788),#1001,.T.);
#7800=ADVANCED_FACE('',(#1308),#1002,.T.);
#7801=ADVANCED_FACE('',(#1309),#1003,.T.);
#7802=ADVANCED_FACE('',(#1310,#789,#790,#791,#792,#793),#1004,.T.);
#7803=ADVANCED_FACE('',(#1311),#1005,.T.);
#7804=ADVANCED_FACE('',(#1312,#794,#795,#796,#797,#798),#1006,.T.);
#7805=ADVANCED_FACE('',(#1313),#1007,.T.);
#7806=ADVANCED_FACE('',(#1314),#1008,.T.);
#7807=ADVANCED_FACE('',(#1315,#799,#800),#1009,.F.);
#7808=ADVANCED_FACE('',(#1316),#7580,.F.);
#7809=ADVANCED_FACE('',(#1317),#7581,.F.);
#7810=ADVANCED_FACE('',(#1318),#7582,.F.);
#7811=ADVANCED_FACE('',(#1319),#7583,.F.);
#7812=ADVANCED_FACE('',(#1320),#7584,.T.);
#7813=ADVANCED_FACE('',(#1321,#801),#1010,.T.);
#7814=ADVANCED_FACE('',(#1322),#7585,.F.);
#7815=ADVANCED_FACE('',(#1323),#7586,.T.);
#7816=ADVANCED_FACE('',(#1324,#802,#803,#804,#805,#806),#1011,.T.);
#7817=ADVANCED_FACE('',(#1325,#807,#808,#809,#810,#811),#1012,.F.);
#7818=ADVANCED_FACE('',(#1326),#7587,.F.);
#7819=ADVANCED_FACE('',(#1327),#7588,.F.);
#7820=ADVANCED_FACE('',(#1328),#7589,.F.);
#7821=ADVANCED_FACE('',(#1329),#7590,.F.);
#7822=ADVANCED_FACE('',(#1330),#7591,.T.);
#7823=ADVANCED_FACE('',(#1331,#812),#1013,.F.);
#7824=ADVANCED_FACE('',(#1332),#7592,.F.);
#7825=ADVANCED_FACE('',(#1333),#7593,.T.);
#7826=ADVANCED_FACE('',(#1334,#813,#814,#815,#816,#817),#1014,.T.);
#7827=ADVANCED_FACE('',(#1335,#818,#819,#820,#821,#822),#1015,.F.);
#7828=ADVANCED_FACE('',(#1336),#7594,.F.);
#7829=ADVANCED_FACE('',(#1337),#7595,.F.);
#7830=ADVANCED_FACE('',(#1338),#7596,.F.);
#7831=ADVANCED_FACE('',(#1339),#7597,.F.);
#7832=ADVANCED_FACE('',(#1340),#7598,.F.);
#7833=ADVANCED_FACE('',(#1341),#7599,.F.);
#7834=ADVANCED_FACE('',(#1342),#7600,.F.);
#7835=ADVANCED_FACE('',(#1343,#823),#1016,.T.);
#7836=ADVANCED_FACE('',(#1344,#824),#1017,.T.);
#7837=ADVANCED_FACE('',(#1345),#1018,.T.);
#7838=ADVANCED_FACE('',(#1346),#1019,.T.);
#7839=ADVANCED_FACE('',(#1347),#1020,.T.);
#7840=ADVANCED_FACE('',(#1348,#825,#826,#827,#828,#829),#1021,.T.);
#7841=ADVANCED_FACE('',(#1349),#1022,.T.);
#7842=ADVANCED_FACE('',(#1350,#830,#831,#832,#833,#834),#1023,.T.);
#7843=ADVANCED_FACE('',(#1351),#1024,.T.);
#7844=ADVANCED_FACE('',(#1352,#835,#836),#1025,.F.);
#7845=ADVANCED_FACE('',(#1353),#7601,.F.);
#7846=ADVANCED_FACE('',(#1354),#7602,.F.);
#7847=ADVANCED_FACE('',(#1355),#7603,.F.);
#7848=ADVANCED_FACE('',(#1356),#7604,.F.);
#7849=ADVANCED_FACE('',(#1357),#7605,.T.);
#7850=ADVANCED_FACE('',(#1358,#837),#1026,.T.);
#7851=ADVANCED_FACE('',(#1359),#7606,.F.);
#7852=ADVANCED_FACE('',(#1360),#7607,.T.);
#7853=ADVANCED_FACE('',(#1361,#838,#839,#840,#841,#842),#1027,.T.);
#7854=ADVANCED_FACE('',(#1362,#843,#844,#845,#846,#847),#1028,.F.);
#7855=ADVANCED_FACE('',(#1363),#7608,.F.);
#7856=ADVANCED_FACE('',(#1364),#7609,.F.);
#7857=ADVANCED_FACE('',(#1365),#7610,.F.);
#7858=ADVANCED_FACE('',(#1366),#7611,.F.);
#7859=ADVANCED_FACE('',(#1367),#7612,.T.);
#7860=ADVANCED_FACE('',(#1368,#848),#1029,.F.);
#7861=ADVANCED_FACE('',(#1369),#7613,.F.);
#7862=ADVANCED_FACE('',(#1370),#7614,.T.);
#7863=ADVANCED_FACE('',(#1371,#849,#850,#851,#852,#853),#1030,.T.);
#7864=ADVANCED_FACE('',(#1372,#854,#855,#856,#857,#858),#1031,.F.);
#7865=ADVANCED_FACE('',(#1373),#7615,.F.);
#7866=ADVANCED_FACE('',(#1374),#7616,.F.);
#7867=ADVANCED_FACE('',(#1375),#7617,.F.);
#7868=ADVANCED_FACE('',(#1376),#7618,.F.);
#7869=ADVANCED_FACE('',(#1377),#7619,.F.);
#7870=ADVANCED_FACE('',(#1378),#7620,.F.);
#7871=ADVANCED_FACE('',(#1379),#7621,.F.);
#7872=ADVANCED_FACE('',(#1380,#859),#1032,.T.);
#7873=ADVANCED_FACE('',(#1381,#860),#1033,.T.);
#7874=ADVANCED_FACE('',(#1382),#1034,.T.);
#7875=ADVANCED_FACE('',(#1383),#1035,.T.);
#7876=ADVANCED_FACE('',(#1384),#1036,.T.);
#7877=ADVANCED_FACE('',(#1385,#861,#862,#863,#864,#865),#1037,.T.);
#7878=ADVANCED_FACE('',(#1386),#1038,.T.);
#7879=ADVANCED_FACE('',(#1387,#866,#867,#868,#869,#870),#1039,.T.);
#7880=ADVANCED_FACE('',(#1388),#1040,.T.);
#7881=ADVANCED_FACE('',(#1389,#871,#872),#1041,.F.);
#7882=ADVANCED_FACE('',(#1390),#7622,.F.);
#7883=ADVANCED_FACE('',(#1391),#7623,.F.);
#7884=ADVANCED_FACE('',(#1392),#7624,.F.);
#7885=ADVANCED_FACE('',(#1393),#7625,.F.);
#7886=ADVANCED_FACE('',(#1394),#7626,.T.);
#7887=ADVANCED_FACE('',(#1395,#873),#1042,.T.);
#7888=ADVANCED_FACE('',(#1396),#7627,.F.);
#7889=ADVANCED_FACE('',(#1397),#7628,.T.);
#7890=ADVANCED_FACE('',(#1398,#874,#875,#876,#877,#878),#1043,.T.);
#7891=ADVANCED_FACE('',(#1399,#879,#880,#881,#882,#883),#1044,.F.);
#7892=ADVANCED_FACE('',(#1400),#7629,.F.);
#7893=ADVANCED_FACE('',(#1401),#7630,.F.);
#7894=ADVANCED_FACE('',(#1402),#7631,.F.);
#7895=ADVANCED_FACE('',(#1403),#7632,.F.);
#7896=ADVANCED_FACE('',(#1404),#7633,.T.);
#7897=ADVANCED_FACE('',(#1405,#884),#1045,.F.);
#7898=ADVANCED_FACE('',(#1406),#7634,.F.);
#7899=ADVANCED_FACE('',(#1407),#7635,.T.);
#7900=ADVANCED_FACE('',(#1408,#885,#886,#887,#888,#889),#1046,.T.);
#7901=ADVANCED_FACE('',(#1409,#890,#891,#892,#893,#894),#1047,.F.);
#7902=ADVANCED_FACE('',(#1410),#7636,.F.);
#7903=ADVANCED_FACE('',(#1411),#7637,.F.);
#7904=ADVANCED_FACE('',(#1412),#7638,.F.);
#7905=ADVANCED_FACE('',(#1413,#895),#1048,.T.);
#7906=ADVANCED_FACE('',(#1414),#7639,.F.);
#7907=ADVANCED_FACE('',(#1415),#7640,.F.);
#7908=ADVANCED_FACE('',(#1416,#896),#1049,.T.);
#7909=ADVANCED_FACE('',(#1417),#7641,.F.);
#7910=ADVANCED_FACE('',(#1418,#897,#898),#1050,.T.);
#7911=ADVANCED_FACE('',(#1419),#1051,.T.);
#7912=ADVANCED_FACE('',(#1420,#899,#900),#1052,.T.);
#7913=ADVANCED_FACE('',(#1421),#1053,.T.);
#7914=ADVANCED_FACE('',(#1422,#901,#902),#1054,.T.);
#7915=ADVANCED_FACE('',(#1423,#903,#904),#1055,.F.);
#7916=ADVANCED_FACE('',(#1424),#7642,.T.);
#7917=ADVANCED_FACE('',(#1425),#1056,.T.);
#7918=ADVANCED_FACE('',(#1426),#1057,.F.);
#7919=ADVANCED_FACE('',(#1427),#7643,.T.);
#7920=ADVANCED_FACE('',(#1428),#1058,.T.);
#7921=ADVANCED_FACE('',(#1429),#1059,.F.);
#7922=ADVANCED_FACE('',(#1430),#515,.T.);
#7923=ADVANCED_FACE('',(#1431),#1060,.T.);
#7924=ADVANCED_FACE('',(#1432),#1061,.F.);
#7925=ADVANCED_FACE('',(#1433),#7644,.T.);
#7926=ADVANCED_FACE('',(#1434),#1062,.T.);
#7927=ADVANCED_FACE('',(#1435),#1063,.F.);
#7928=ADVANCED_FACE('',(#1436),#7645,.T.);
#7929=ADVANCED_FACE('',(#1437),#1064,.T.);
#7930=ADVANCED_FACE('',(#1438),#1065,.F.);
#7931=ADVANCED_FACE('',(#1439),#516,.T.);
#7932=ADVANCED_FACE('',(#1440),#1066,.T.);
#7933=ADVANCED_FACE('',(#1441),#1067,.F.);
#7934=ADVANCED_FACE('',(#1442),#1068,.T.);
#7935=ADVANCED_FACE('',(#1443),#455,.T.);
#7936=ADVANCED_FACE('',(#1444),#7646,.T.);
#7937=ADVANCED_FACE('',(#1445),#456,.T.);
#7938=ADVANCED_FACE('',(#1446,#905),#1069,.T.);
#7939=ADVANCED_FACE('',(#1447),#457,.T.);
#7940=ADVANCED_FACE('',(#1448),#7647,.T.);
#7941=ADVANCED_FACE('',(#1449),#458,.T.);
#7942=ADVANCED_FACE('',(#1450),#1070,.T.);
#7943=ADVANCED_FACE('',(#1451),#1071,.F.);
#7944=ADVANCED_FACE('',(#1452),#1072,.F.);
#7945=ADVANCED_FACE('',(#1453),#1073,.F.);
#7946=ADVANCED_FACE('',(#1454),#1074,.F.);
#7947=ADVANCED_FACE('',(#1455),#1075,.F.);
#7948=ADVANCED_FACE('',(#1456),#1076,.F.);
#7949=ADVANCED_FACE('',(#1457),#1077,.F.);
#7950=ADVANCED_FACE('',(#1458),#1078,.F.);
#7951=ADVANCED_FACE('',(#1459),#449,.F.);
#7952=ADVANCED_FACE('',(#1460),#7648,.T.);
#7953=ADVANCED_FACE('',(#1461),#7649,.F.);
#7954=ADVANCED_FACE('',(#1462),#459,.F.);
#7955=ADVANCED_FACE('',(#1463,#906),#1079,.T.);
#7956=ADVANCED_FACE('',(#1464),#7650,.T.);
#7957=ADVANCED_FACE('',(#1465,#907),#1080,.T.);
#7958=ADVANCED_FACE('',(#1466),#460,.F.);
#7959=ADVANCED_FACE('',(#1467),#450,.F.);
#7960=ADVANCED_FACE('',(#1468),#7651,.F.);
#7961=ADVANCED_FACE('',(#1469,#908),#1081,.T.);
#7962=ADVANCED_FACE('',(#1470),#461,.T.);
#7963=ADVANCED_FACE('',(#1471),#7652,.T.);
#7964=ADVANCED_FACE('',(#1472),#462,.T.);
#7965=ADVANCED_FACE('',(#1473,#909),#1082,.T.);
#7966=ADVANCED_FACE('',(#1474),#7653,.F.);
#7967=ADVANCED_FACE('',(#1475),#435,.T.);
#7968=ADVANCED_FACE('',(#1476),#436,.T.);
#7969=ADVANCED_FACE('',(#1477),#437,.T.);
#7970=ADVANCED_FACE('',(#1478),#438,.T.);
#7971=ADVANCED_FACE('',(#1479),#439,.T.);
#7972=ADVANCED_FACE('',(#1480),#440,.T.);
#7973=ADVANCED_FACE('',(#1481),#441,.T.);
#7974=ADVANCED_FACE('',(#1482),#442,.F.);
#7975=ADVANCED_FACE('',(#1483),#7654,.T.);
#7976=ADVANCED_FACE('',(#1484),#1083,.T.);
#7977=ADVANCED_FACE('',(#1485),#443,.F.);
#7978=ADVANCED_FACE('',(#1486),#1084,.T.);
#7979=ADVANCED_FACE('',(#1487),#444,.F.);
#7980=ADVANCED_FACE('',(#1488),#1085,.T.);
#7981=ADVANCED_FACE('',(#1489),#445,.F.);
#7982=ADVANCED_FACE('',(#1490),#1086,.T.);
#7983=ADVANCED_FACE('',(#1491),#446,.F.);
#7984=ADVANCED_FACE('',(#1492),#1087,.T.);
#7985=ADVANCED_FACE('',(#1493),#447,.F.);
#7986=ADVANCED_FACE('',(#1494),#7655,.F.);
#7987=ADVANCED_FACE('',(#1495),#1088,.T.);
#7988=ADVANCED_FACE('',(#1496),#448,.F.);
#7989=ADVANCED_FACE('',(#1497,#910),#1089,.T.);
#7990=ADVANCED_FACE('',(#1498),#1090,.T.);
#7991=ADVANCED_FACE('',(#1499,#911),#1091,.T.);
#7992=ADVANCED_FACE('',(#1500),#7656,.T.);
#7993=ADVANCED_FACE('',(#1501,#912),#1092,.T.);
#7994=ADVANCED_FACE('',(#1502),#7657,.F.);
#7995=ADVANCED_FACE('',(#1503,#913),#1093,.T.);
#7996=ADVANCED_FACE('',(#1504),#7658,.T.);
#7997=ADVANCED_FACE('',(#1505,#914),#1094,.T.);
#7998=ADVANCED_FACE('',(#1506),#7659,.F.);
#7999=ADVANCED_FACE('',(#1507),#1095,.F.);
#8000=ADVANCED_FACE('',(#1508),#1096,.F.);
#8001=ADVANCED_FACE('',(#1509),#1097,.F.);
#8002=ADVANCED_FACE('',(#1510),#1098,.F.);
#8003=ADVANCED_FACE('',(#1511),#1099,.F.);
#8004=ADVANCED_FACE('',(#1512),#1100,.F.);
#8005=ADVANCED_FACE('',(#1513),#1101,.F.);
#8006=ADVANCED_FACE('',(#1514),#1102,.F.);
#8007=ADVANCED_FACE('',(#1515),#1103,.F.);
#8008=ADVANCED_FACE('',(#1516),#1104,.T.);
#8009=ADVANCED_FACE('',(#1517),#463,.T.);
#8010=ADVANCED_FACE('',(#1518),#7660,.T.);
#8011=ADVANCED_FACE('',(#1519),#464,.T.);
#8012=ADVANCED_FACE('',(#1520,#915),#1105,.T.);
#8013=ADVANCED_FACE('',(#1521),#465,.T.);
#8014=ADVANCED_FACE('',(#1522),#7661,.T.);
#8015=ADVANCED_FACE('',(#1523),#1106,.T.);
#8016=ADVANCED_FACE('',(#1524),#466,.T.);
#8017=ADVANCED_FACE('',(#1525),#7662,.T.);
#8018=ADVANCED_FACE('',(#1526),#467,.T.);
#8019=ADVANCED_FACE('',(#1527,#916),#1107,.T.);
#8020=ADVANCED_FACE('',(#1528),#468,.T.);
#8021=ADVANCED_FACE('',(#1529),#7663,.T.);
#8022=ADVANCED_FACE('',(#1530),#469,.T.);
#8023=ADVANCED_FACE('',(#1531),#1108,.T.);
#8024=ADVANCED_FACE('',(#1532),#1109,.F.);
#8025=ADVANCED_FACE('',(#1533),#1110,.F.);
#8026=ADVANCED_FACE('',(#1534),#1111,.F.);
#8027=ADVANCED_FACE('',(#1535),#1112,.F.);
#8028=ADVANCED_FACE('',(#1536),#1113,.F.);
#8029=ADVANCED_FACE('',(#1537),#1114,.F.);
#8030=ADVANCED_FACE('',(#1538),#1115,.F.);
#8031=ADVANCED_FACE('',(#1539),#1116,.F.);
#8032=ADVANCED_FACE('',(#1540),#470,.T.);
#8033=ADVANCED_FACE('',(#1541),#471,.T.);
#8034=ADVANCED_FACE('',(#1542),#1117,.T.);
#8035=ADVANCED_FACE('',(#1543),#1118,.T.);
#8036=ADVANCED_FACE('',(#1544),#1119,.T.);
#8037=ADVANCED_FACE('',(#1545),#7664,.F.);
#8038=ADVANCED_FACE('',(#1546),#1120,.T.);
#8039=ADVANCED_FACE('',(#1547),#1121,.T.);
#8040=ADVANCED_FACE('',(#1548),#1122,.T.);
#8041=ADVANCED_FACE('',(#1549,#917),#1123,.T.);
#8042=ADVANCED_FACE('',(#1550,#918),#1124,.F.);
#8043=ADVANCED_FACE('',(#1551),#7665,.F.);
#8044=ADVANCED_FACE('',(#1552),#1125,.T.);
#8045=ADVANCED_FACE('',(#1553),#1126,.F.);
#8046=ADVANCED_FACE('',(#1554),#1127,.T.);
#8047=ADVANCED_FACE('',(#1555),#1128,.F.);
#8048=ADVANCED_FACE('',(#1556),#1129,.F.);
#8049=ADVANCED_FACE('',(#1557),#1130,.F.);
#8050=ADVANCED_FACE('',(#1558,#919),#1131,.T.);
#8051=ADVANCED_FACE('',(#1559,#920),#1132,.F.);
#8052=ADVANCED_FACE('',(#1560),#7666,.T.);
#8053=ADVANCED_FACE('',(#1561),#7667,.T.);
#8054=ADVANCED_FACE('',(#1562,#921),#7668,.T.);
#8055=ADVANCED_FACE('',(#1563,#922),#1133,.T.);
#8056=ADVANCED_FACE('',(#1564),#1134,.F.);
#8057=ADVANCED_FACE('',(#1565),#7669,.F.);
#8058=ADVANCED_FACE('',(#1566),#7670,.T.);
#8059=ADVANCED_FACE('',(#1567,#923),#1135,.T.);
#8060=ADVANCED_FACE('',(#1568,#924),#1136,.F.);
#8061=ADVANCED_FACE('',(#1569),#1137,.T.);
#8062=ADVANCED_FACE('',(#1570),#7671,.F.);
#8063=ADVANCED_FACE('',(#1571),#1138,.T.);
#8064=ADVANCED_FACE('',(#1572,#925),#7672,.F.);
#8065=ADVANCED_FACE('',(#1573,#926),#7673,.T.);
#8066=ADVANCED_FACE('',(#1574,#927),#1139,.T.);
#8067=ADVANCED_FACE('',(#1575,#928),#1140,.F.);
#8068=ADVANCED_FACE('',(#1576),#1141,.F.);
#8069=ADVANCED_FACE('',(#1577),#1142,.F.);
#8070=ADVANCED_FACE('',(#1578),#1143,.F.);
#8071=ADVANCED_FACE('',(#1579,#929),#1144,.T.);
#8072=ADVANCED_FACE('',(#1580),#7674,.F.);
#8073=ADVANCED_FACE('',(#1581,#930),#1145,.F.);
#8074=ADVANCED_FACE('',(#1582),#7675,.T.);
#8075=ADVANCED_FACE('',(#1583),#7676,.T.);
#8076=ADVANCED_FACE('',(#1584,#931),#1146,.F.);
#8077=ADVANCED_FACE('',(#1585),#7677,.F.);
#8078=ADVANCED_FACE('',(#1586),#7678,.T.);
#8079=ADVANCED_FACE('',(#1587,#932),#1147,.T.);
#8080=ADVANCED_FACE('',(#1588,#933),#1148,.F.);
#8081=ADVANCED_FACE('',(#1589),#7679,.F.);
#8082=ADVANCED_FACE('',(#1590),#7680,.T.);
#8083=ADVANCED_FACE('',(#1591,#934),#1149,.T.);
#8084=ADVANCED_FACE('',(#1592,#935),#1150,.F.);
#8085=ADVANCED_FACE('',(#1593),#1151,.T.);
#8086=ADVANCED_FACE('',(#1594),#472,.T.);
#8087=ADVANCED_FACE('',(#1595),#7681,.T.);
#8088=ADVANCED_FACE('',(#1596),#473,.T.);
#8089=ADVANCED_FACE('',(#1597,#936),#1152,.T.);
#8090=ADVANCED_FACE('',(#1598),#474,.T.);
#8091=ADVANCED_FACE('',(#1599),#7682,.T.);
#8092=ADVANCED_FACE('',(#1600),#475,.T.);
#8093=ADVANCED_FACE('',(#1601),#1153,.T.);
#8094=ADVANCED_FACE('',(#1602),#1154,.F.);
#8095=ADVANCED_FACE('',(#1603),#1155,.F.);
#8096=ADVANCED_FACE('',(#1604),#1156,.F.);
#8097=ADVANCED_FACE('',(#1605),#1157,.F.);
#8098=ADVANCED_FACE('',(#1606),#1158,.F.);
#8099=ADVANCED_FACE('',(#1607),#1159,.F.);
#8100=ADVANCED_FACE('',(#1608),#1160,.F.);
#8101=ADVANCED_FACE('',(#1609),#1161,.F.);
#8102=ADVANCED_FACE('',(#1610),#1162,.F.);
#8103=ADVANCED_FACE('',(#1611),#1163,.T.);
#8104=ADVANCED_FACE('',(#1612),#1164,.F.);
#8105=ADVANCED_FACE('',(#1613),#1165,.F.);
#8106=ADVANCED_FACE('',(#1614),#1166,.F.);
#8107=ADVANCED_FACE('',(#1615,#937),#1167,.T.);
#8108=ADVANCED_FACE('',(#1616,#938),#1168,.F.);
#8109=ADVANCED_FACE('',(#1617),#7683,.T.);
#8110=ADVANCED_FACE('',(#1618),#7684,.T.);
#8111=ADVANCED_FACE('',(#1619,#939),#7685,.T.);
#8112=ADVANCED_FACE('',(#1620),#1169,.T.);
#8113=ADVANCED_FACE('',(#1621),#1170,.F.);
#8114=ADVANCED_FACE('',(#1622),#1171,.F.);
#8115=ADVANCED_FACE('',(#1623),#1172,.F.);
#8116=ADVANCED_FACE('',(#1624),#1173,.F.);
#8117=ADVANCED_FACE('',(#1625,#940),#1174,.T.);
#8118=ADVANCED_FACE('',(#1626),#7686,.F.);
#8119=ADVANCED_FACE('',(#1627,#941),#1175,.T.);
#8120=ADVANCED_FACE('',(#1628),#7687,.T.);
#8121=ADVANCED_FACE('',(#1629),#7688,.T.);
#8122=ADVANCED_FACE('',(#1630,#942),#1176,.F.);
#8123=ADVANCED_FACE('',(#1631),#7689,.F.);
#8124=ADVANCED_FACE('',(#1632),#7690,.T.);
#8125=ADVANCED_FACE('',(#1633,#943),#1177,.T.);
#8126=ADVANCED_FACE('',(#1634,#944),#1178,.F.);
#8127=ADVANCED_FACE('',(#1635),#7691,.F.);
#8128=ADVANCED_FACE('',(#1636),#7692,.T.);
#8129=ADVANCED_FACE('',(#1637,#945),#1179,.T.);
#8130=ADVANCED_FACE('',(#1638,#946),#1180,.F.);
#8131=ADVANCED_FACE('',(#1639),#1181,.T.);
#8132=ADVANCED_FACE('',(#1640),#7693,.F.);
#8133=ADVANCED_FACE('',(#1641),#1182,.T.);
#8134=ADVANCED_FACE('',(#1642),#7694,.F.);
#8135=ADVANCED_FACE('',(#1643),#7695,.T.);
#8136=ADVANCED_FACE('',(#1644,#947),#1183,.T.);
#8137=ADVANCED_FACE('',(#1645,#948),#1184,.F.);
#8138=ADVANCED_FACE('',(#1646),#1185,.T.);
#8139=ADVANCED_FACE('',(#1647),#7696,.F.);
#8140=ADVANCED_FACE('',(#1648),#1186,.T.);
#8141=ADVANCED_FACE('',(#1649),#7697,.F.);
#8142=ADVANCED_FACE('',(#1650),#7698,.T.);
#8143=ADVANCED_FACE('',(#1651,#949),#1187,.T.);
#8144=ADVANCED_FACE('',(#1652,#950),#1188,.F.);
#8145=ADVANCED_FACE('',(#1653),#1189,.T.);
#8146=ADVANCED_FACE('',(#1654),#1190,.T.);
#8147=ADVANCED_FACE('',(#1655),#1191,.T.);
#8148=ADVANCED_FACE('',(#1656),#1192,.T.);
#8149=ADVANCED_FACE('',(#1657),#1193,.T.);
#8150=ADVANCED_FACE('',(#1658),#1194,.F.);
#8151=ADVANCED_FACE('',(#1659),#1195,.T.);
#8152=ADVANCED_FACE('',(#1660),#1196,.T.);
#8153=ADVANCED_FACE('',(#1661),#1197,.T.);
#8154=ADVANCED_FACE('',(#1662),#1198,.F.);
#8155=ADVANCED_FACE('',(#1663),#1199,.F.);
#8156=ADVANCED_FACE('',(#1664),#1200,.F.);
#8157=ADVANCED_FACE('',(#1665),#1201,.F.);
#8158=ADVANCED_FACE('',(#1666),#1202,.F.);
#8159=ADVANCED_FACE('',(#1667),#1203,.F.);
#8160=ADVANCED_FACE('',(#1668),#1204,.F.);
#8161=ADVANCED_FACE('',(#1669),#1205,.F.);
#8162=ADVANCED_FACE('',(#1670),#1206,.F.);
#8163=ADVANCED_FACE('',(#1671,#951),#1207,.T.);
#8164=ADVANCED_FACE('',(#1672),#476,.T.);
#8165=ADVANCED_FACE('',(#1673),#7699,.T.);
#8166=CLOSED_SHELL('',(#7700,#7701,#7702,#7703,#7704,#7705,#7706,#7707,
#7708,#7709,#7710,#7711,#7712,#7713,#7714,#7715));
#8167=CLOSED_SHELL('',(#7716,#7717,#7718,#7719,#7720,#7721));
#8168=CLOSED_SHELL('',(#7722,#7723,#7724,#7725,#7726,#7727));
#8169=CLOSED_SHELL('',(#7728,#7729,#7730,#7731,#7732,#7733,#7734,#7735,
#7736,#7737,#7738,#7739,#7740,#7741,#7742,#7743,#7744,#7745,#7746,#7747,
#7748,#7749,#7750,#7751,#7752,#7753));
#8170=CLOSED_SHELL('',(#7754,#7755,#7756,#7757,#7758,#7759,#7760,#7761,
#7762,#7763,#7764,#7765,#7766,#7767,#7768,#7769,#7770));
#8171=CLOSED_SHELL('',(#7771,#7772,#7773,#7774,#7775,#7776,#7777,#7778,
#7779,#7780));
#8172=CLOSED_SHELL('',(#7781,#7782,#7783,#7784,#7785,#7786,#7787,#7788,
#7789,#7790));
#8173=CLOSED_SHELL('',(#7791,#7792,#7793,#7794,#7795,#7796,#7797,#7798,
#7799,#7800,#7801,#7802,#7803,#7804,#7805,#7806,#7807));
#8174=CLOSED_SHELL('',(#7808,#7809,#7810,#7811,#7812,#7813,#7814,#7815,
#7816,#7817));
#8175=CLOSED_SHELL('',(#7818,#7819,#7820,#7821,#7822,#7823,#7824,#7825,
#7826,#7827));
#8176=CLOSED_SHELL('',(#7828,#7829,#7830,#7831,#7832,#7833,#7834,#7835,
#7836,#7837,#7838,#7839,#7840,#7841,#7842,#7843,#7844));
#8177=CLOSED_SHELL('',(#7845,#7846,#7847,#7848,#7849,#7850,#7851,#7852,
#7853,#7854));
#8178=CLOSED_SHELL('',(#7855,#7856,#7857,#7858,#7859,#7860,#7861,#7862,
#7863,#7864));
#8179=CLOSED_SHELL('',(#7865,#7866,#7867,#7868,#7869,#7870,#7871,#7872,
#7873,#7874,#7875,#7876,#7877,#7878,#7879,#7880,#7881));
#8180=CLOSED_SHELL('',(#7882,#7883,#7884,#7885,#7886,#7887,#7888,#7889,
#7890,#7891));
#8181=CLOSED_SHELL('',(#7892,#7893,#7894,#7895,#7896,#7897,#7898,#7899,
#7900,#7901));
#8182=CLOSED_SHELL('',(#7902,#7903,#7904,#7905,#7906,#7907,#7908,#7909,
#7910,#7911,#7912,#7913,#7914,#7915));
#8183=CLOSED_SHELL('',(#7916,#7917,#7918));
#8184=CLOSED_SHELL('',(#7919,#7920,#7921));
#8185=CLOSED_SHELL('',(#7922,#7923,#7924));
#8186=CLOSED_SHELL('',(#7925,#7926,#7927));
#8187=CLOSED_SHELL('',(#7928,#7929,#7930));
#8188=CLOSED_SHELL('',(#7931,#7932,#7933));
#8189=CLOSED_SHELL('',(#7934,#7935,#7936,#7937,#7938,#7939,#7940,#7941,
#7942));
#8190=CLOSED_SHELL('',(#7943,#7944,#7945,#7946,#7947,#7948,#7949,#7950));
#8191=CLOSED_SHELL('',(#7951,#7952,#7953,#7954,#7955,#7956,#7957,#7958));
#8192=CLOSED_SHELL('',(#7959,#7960,#7961,#7962,#7963,#7964,#7965,#7966));
#8193=CLOSED_SHELL('',(#7967));
#8194=CLOSED_SHELL('',(#7968));
#8195=CLOSED_SHELL('',(#7969));
#8196=CLOSED_SHELL('',(#7970));
#8197=CLOSED_SHELL('',(#7971));
#8198=CLOSED_SHELL('',(#7972));
#8199=CLOSED_SHELL('',(#7973));
#8200=CLOSED_SHELL('',(#7974,#7975,#7976,#7977,#7978,#7979,#7980,#7981,
#7982,#7983,#7984,#7985,#7986,#7987,#7988,#7989,#7990));
#8201=CLOSED_SHELL('',(#7991,#7992,#7993,#7994));
#8202=CLOSED_SHELL('',(#7995,#7996,#7997,#7998));
#8203=CLOSED_SHELL('',(#7999,#8000,#8001,#8002,#8003,#8004,#8005,#8006));
#8204=CLOSED_SHELL('',(#8007,#8008,#8009,#8010,#8011,#8012,#8013,#8014));
#8205=CLOSED_SHELL('',(#8015,#8016,#8017,#8018,#8019,#8020,#8021,#8022,
#8023));
#8206=CLOSED_SHELL('',(#8024,#8025,#8026,#8027,#8028,#8029,#8030,#8031));
#8207=CLOSED_SHELL('',(#8032,#8033,#8034,#8035,#8036,#8037,#8038,#8039,
#8040,#8041,#8042));
#8208=CLOSED_SHELL('',(#8043,#8044,#8045,#8046,#8047,#8048,#8049,#8050,
#8051,#8052,#8053,#8054,#8055,#8056));
#8209=CLOSED_SHELL('',(#8057,#8058,#8059,#8060));
#8210=CLOSED_SHELL('',(#8061,#8062,#8063,#8064,#8065,#8066,#8067));
#8211=CLOSED_SHELL('',(#8068,#8069,#8070,#8071,#8072,#8073,#8074,#8075,
#8076));
#8212=CLOSED_SHELL('',(#8077,#8078,#8079,#8080));
#8213=CLOSED_SHELL('',(#8081,#8082,#8083,#8084));
#8214=CLOSED_SHELL('',(#8085,#8086,#8087,#8088,#8089,#8090,#8091,#8092,
#8093));
#8215=CLOSED_SHELL('',(#8094,#8095,#8096,#8097,#8098,#8099,#8100,#8101));
#8216=CLOSED_SHELL('',(#8102,#8103,#8104,#8105,#8106,#8107,#8108,#8109,
#8110,#8111,#8112,#8113));
#8217=CLOSED_SHELL('',(#8114,#8115,#8116,#8117,#8118,#8119,#8120,#8121,
#8122));
#8218=CLOSED_SHELL('',(#8123,#8124,#8125,#8126));
#8219=CLOSED_SHELL('',(#8127,#8128,#8129,#8130));
#8220=CLOSED_SHELL('',(#8131,#8132,#8133,#8134,#8135,#8136,#8137));
#8221=CLOSED_SHELL('',(#8138,#8139,#8140,#8141,#8142,#8143,#8144));
#8222=CLOSED_SHELL('',(#8145,#8146,#8147,#8148,#8149,#8150,#8151,#8152,
#8153,#8154));
#8223=CLOSED_SHELL('',(#8155,#8156,#8157,#8158,#8159,#8160,#8161,#8162,
#8163,#8164,#8165));
#8224=DERIVED_UNIT_ELEMENT(#8318,1.);
#8225=DERIVED_UNIT_ELEMENT(#17048,-3.);
#8226=DERIVED_UNIT_ELEMENT(#8318,1.);
#8227=DERIVED_UNIT_ELEMENT(#17048,-3.);
#8228=DERIVED_UNIT_ELEMENT(#8318,1.);
#8229=DERIVED_UNIT_ELEMENT(#17048,-3.);
#8230=DERIVED_UNIT_ELEMENT(#8318,1.);
#8231=DERIVED_UNIT_ELEMENT(#17048,-3.);
#8232=DERIVED_UNIT_ELEMENT(#8318,1.);
#8233=DERIVED_UNIT_ELEMENT(#17048,-3.);
#8234=DERIVED_UNIT_ELEMENT(#8318,1.);
#8235=DERIVED_UNIT_ELEMENT(#17048,-3.);
#8236=DERIVED_UNIT_ELEMENT(#8318,1.);
#8237=DERIVED_UNIT_ELEMENT(#17048,-3.);
#8238=DERIVED_UNIT_ELEMENT(#8318,1.);
#8239=DERIVED_UNIT_ELEMENT(#17048,-3.);
#8240=DERIVED_UNIT_ELEMENT(#8318,1.);
#8241=DERIVED_UNIT_ELEMENT(#17048,-3.);
#8242=DERIVED_UNIT_ELEMENT(#8318,1.);
#8243=DERIVED_UNIT_ELEMENT(#17048,-3.);
#8244=DERIVED_UNIT_ELEMENT(#8318,1.);
#8245=DERIVED_UNIT_ELEMENT(#17048,-3.);
#8246=DERIVED_UNIT_ELEMENT(#8318,1.);
#8247=DERIVED_UNIT_ELEMENT(#17048,-3.);
#8248=DERIVED_UNIT_ELEMENT(#8318,1.);
#8249=DERIVED_UNIT_ELEMENT(#17048,-3.);
#8250=DERIVED_UNIT_ELEMENT(#8318,1.);
#8251=DERIVED_UNIT_ELEMENT(#17048,-3.);
#8252=DERIVED_UNIT_ELEMENT(#8318,1.);
#8253=DERIVED_UNIT_ELEMENT(#17048,-3.);
#8254=DERIVED_UNIT_ELEMENT(#8318,1.);
#8255=DERIVED_UNIT_ELEMENT(#17048,-3.);
#8256=DERIVED_UNIT_ELEMENT(#8318,1.);
#8257=DERIVED_UNIT_ELEMENT(#17048,-3.);
#8258=DERIVED_UNIT_ELEMENT(#8318,1.);
#8259=DERIVED_UNIT_ELEMENT(#17048,-3.);
#8260=DERIVED_UNIT_ELEMENT(#8318,1.);
#8261=DERIVED_UNIT_ELEMENT(#17048,-3.);
#8262=DERIVED_UNIT_ELEMENT(#8318,1.);
#8263=DERIVED_UNIT_ELEMENT(#17048,-3.);
#8264=DERIVED_UNIT_ELEMENT(#8318,1.);
#8265=DERIVED_UNIT_ELEMENT(#17048,-3.);
#8266=DERIVED_UNIT_ELEMENT(#8318,1.);
#8267=DERIVED_UNIT_ELEMENT(#17048,-3.);
#8268=DERIVED_UNIT_ELEMENT(#8318,1.);
#8269=DERIVED_UNIT_ELEMENT(#17048,-3.);
#8270=DERIVED_UNIT_ELEMENT(#8318,1.);
#8271=DERIVED_UNIT_ELEMENT(#17048,-3.);
#8272=DERIVED_UNIT_ELEMENT(#8318,1.);
#8273=DERIVED_UNIT_ELEMENT(#17048,-3.);
#8274=DERIVED_UNIT_ELEMENT(#8318,1.);
#8275=DERIVED_UNIT_ELEMENT(#17048,-3.);
#8276=DERIVED_UNIT_ELEMENT(#8318,1.);
#8277=DERIVED_UNIT_ELEMENT(#17048,-3.);
#8278=DERIVED_UNIT_ELEMENT(#8318,1.);
#8279=DERIVED_UNIT_ELEMENT(#17048,-3.);
#8280=DERIVED_UNIT_ELEMENT(#8318,1.);
#8281=DERIVED_UNIT_ELEMENT(#17048,-3.);
#8282=DERIVED_UNIT_ELEMENT(#8318,1.);
#8283=DERIVED_UNIT_ELEMENT(#17048,-3.);
#8284=DERIVED_UNIT_ELEMENT(#8318,1.);
#8285=DERIVED_UNIT_ELEMENT(#17048,-3.);
#8286=DERIVED_UNIT_ELEMENT(#8318,1.);
#8287=DERIVED_UNIT_ELEMENT(#17048,-3.);
#8288=DERIVED_UNIT_ELEMENT(#8318,1.);
#8289=DERIVED_UNIT_ELEMENT(#17048,-3.);
#8290=DERIVED_UNIT_ELEMENT(#8318,1.);
#8291=DERIVED_UNIT_ELEMENT(#17048,-3.);
#8292=DERIVED_UNIT_ELEMENT(#8318,1.);
#8293=DERIVED_UNIT_ELEMENT(#17048,-3.);
#8294=DERIVED_UNIT_ELEMENT(#8318,1.);
#8295=DERIVED_UNIT_ELEMENT(#17048,-3.);
#8296=DERIVED_UNIT_ELEMENT(#8318,1.);
#8297=DERIVED_UNIT_ELEMENT(#17048,-3.);
#8298=DERIVED_UNIT_ELEMENT(#8318,1.);
#8299=DERIVED_UNIT_ELEMENT(#17048,-3.);
#8300=DERIVED_UNIT_ELEMENT(#8318,1.);
#8301=DERIVED_UNIT_ELEMENT(#17048,-3.);
#8302=DERIVED_UNIT_ELEMENT(#8318,1.);
#8303=DERIVED_UNIT_ELEMENT(#17048,-3.);
#8304=DERIVED_UNIT_ELEMENT(#8318,1.);
#8305=DERIVED_UNIT_ELEMENT(#17048,-3.);
#8306=DERIVED_UNIT_ELEMENT(#8318,1.);
#8307=DERIVED_UNIT_ELEMENT(#17048,-3.);
#8308=DERIVED_UNIT_ELEMENT(#8318,1.);
#8309=DERIVED_UNIT_ELEMENT(#17048,-3.);
#8310=DERIVED_UNIT_ELEMENT(#8318,1.);
#8311=DERIVED_UNIT_ELEMENT(#17048,-3.);
#8312=DERIVED_UNIT_ELEMENT(#8318,1.);
#8313=DERIVED_UNIT_ELEMENT(#17048,-3.);
#8314=DERIVED_UNIT_ELEMENT(#8318,1.);
#8315=DERIVED_UNIT_ELEMENT(#17048,-3.);
#8316=DERIVED_UNIT_ELEMENT(#8318,1.);
#8317=DERIVED_UNIT_ELEMENT(#17048,-3.);
#8318=(
MASS_UNIT()
NAMED_UNIT(*)
SI_UNIT(.KILO.,.GRAM.)
);
#8319=DERIVED_UNIT((#8224,#8225));
#8320=DERIVED_UNIT((#8226,#8227));
#8321=DERIVED_UNIT((#8228,#8229));
#8322=DERIVED_UNIT((#8230,#8231));
#8323=DERIVED_UNIT((#8232,#8233));
#8324=DERIVED_UNIT((#8234,#8235));
#8325=DERIVED_UNIT((#8236,#8237));
#8326=DERIVED_UNIT((#8238,#8239));
#8327=DERIVED_UNIT((#8240,#8241));
#8328=DERIVED_UNIT((#8242,#8243));
#8329=DERIVED_UNIT((#8244,#8245));
#8330=DERIVED_UNIT((#8246,#8247));
#8331=DERIVED_UNIT((#8248,#8249));
#8332=DERIVED_UNIT((#8250,#8251));
#8333=DERIVED_UNIT((#8252,#8253));
#8334=DERIVED_UNIT((#8254,#8255));
#8335=DERIVED_UNIT((#8256,#8257));
#8336=DERIVED_UNIT((#8258,#8259));
#8337=DERIVED_UNIT((#8260,#8261));
#8338=DERIVED_UNIT((#8262,#8263));
#8339=DERIVED_UNIT((#8264,#8265));
#8340=DERIVED_UNIT((#8266,#8267));
#8341=DERIVED_UNIT((#8268,#8269));
#8342=DERIVED_UNIT((#8270,#8271));
#8343=DERIVED_UNIT((#8272,#8273));
#8344=DERIVED_UNIT((#8274,#8275));
#8345=DERIVED_UNIT((#8276,#8277));
#8346=DERIVED_UNIT((#8278,#8279));
#8347=DERIVED_UNIT((#8280,#8281));
#8348=DERIVED_UNIT((#8282,#8283));
#8349=DERIVED_UNIT((#8284,#8285));
#8350=DERIVED_UNIT((#8286,#8287));
#8351=DERIVED_UNIT((#8288,#8289));
#8352=DERIVED_UNIT((#8290,#8291));
#8353=DERIVED_UNIT((#8292,#8293));
#8354=DERIVED_UNIT((#8294,#8295));
#8355=DERIVED_UNIT((#8296,#8297));
#8356=DERIVED_UNIT((#8298,#8299));
#8357=DERIVED_UNIT((#8300,#8301));
#8358=DERIVED_UNIT((#8302,#8303));
#8359=DERIVED_UNIT((#8304,#8305));
#8360=DERIVED_UNIT((#8306,#8307));
#8361=DERIVED_UNIT((#8308,#8309));
#8362=DERIVED_UNIT((#8310,#8311));
#8363=DERIVED_UNIT((#8312,#8313));
#8364=DERIVED_UNIT((#8314,#8315));
#8365=DERIVED_UNIT((#8316,#8317));
#8366=MEASURE_REPRESENTATION_ITEM('density measure',
POSITIVE_RATIO_MEASURE(7850.),#8319);
#8367=MEASURE_REPRESENTATION_ITEM('density measure',
POSITIVE_RATIO_MEASURE(7850.),#8320);
#8368=MEASURE_REPRESENTATION_ITEM('density measure',
POSITIVE_RATIO_MEASURE(7850.),#8321);
#8369=MEASURE_REPRESENTATION_ITEM('density measure',
POSITIVE_RATIO_MEASURE(7850.),#8322);
#8370=MEASURE_REPRESENTATION_ITEM('density measure',
POSITIVE_RATIO_MEASURE(7850.),#8323);
#8371=MEASURE_REPRESENTATION_ITEM('density measure',
POSITIVE_RATIO_MEASURE(7850.),#8324);
#8372=MEASURE_REPRESENTATION_ITEM('density measure',
POSITIVE_RATIO_MEASURE(7850.),#8325);
#8373=MEASURE_REPRESENTATION_ITEM('density measure',
POSITIVE_RATIO_MEASURE(7850.),#8326);
#8374=MEASURE_REPRESENTATION_ITEM('density measure',
POSITIVE_RATIO_MEASURE(7850.),#8327);
#8375=MEASURE_REPRESENTATION_ITEM('density measure',
POSITIVE_RATIO_MEASURE(7850.),#8328);
#8376=MEASURE_REPRESENTATION_ITEM('density measure',
POSITIVE_RATIO_MEASURE(7850.),#8329);
#8377=MEASURE_REPRESENTATION_ITEM('density measure',
POSITIVE_RATIO_MEASURE(7850.),#8330);
#8378=MEASURE_REPRESENTATION_ITEM('density measure',
POSITIVE_RATIO_MEASURE(7850.),#8331);
#8379=MEASURE_REPRESENTATION_ITEM('density measure',
POSITIVE_RATIO_MEASURE(7850.),#8332);
#8380=MEASURE_REPRESENTATION_ITEM('density measure',
POSITIVE_RATIO_MEASURE(7850.),#8333);
#8381=MEASURE_REPRESENTATION_ITEM('density measure',
POSITIVE_RATIO_MEASURE(7850.),#8334);
#8382=MEASURE_REPRESENTATION_ITEM('density measure',
POSITIVE_RATIO_MEASURE(7850.),#8335);
#8383=MEASURE_REPRESENTATION_ITEM('density measure',
POSITIVE_RATIO_MEASURE(7850.),#8336);
#8384=MEASURE_REPRESENTATION_ITEM('density measure',
POSITIVE_RATIO_MEASURE(7850.),#8337);
#8385=MEASURE_REPRESENTATION_ITEM('density measure',
POSITIVE_RATIO_MEASURE(7850.),#8338);
#8386=MEASURE_REPRESENTATION_ITEM('density measure',
POSITIVE_RATIO_MEASURE(7850.),#8339);
#8387=MEASURE_REPRESENTATION_ITEM('density measure',
POSITIVE_RATIO_MEASURE(7850.),#8340);
#8388=MEASURE_REPRESENTATION_ITEM('density measure',
POSITIVE_RATIO_MEASURE(7850.),#8341);
#8389=MEASURE_REPRESENTATION_ITEM('density measure',
POSITIVE_RATIO_MEASURE(7850.),#8342);
#8390=MEASURE_REPRESENTATION_ITEM('density measure',
POSITIVE_RATIO_MEASURE(7850.),#8343);
#8391=MEASURE_REPRESENTATION_ITEM('density measure',
POSITIVE_RATIO_MEASURE(7850.),#8344);
#8392=MEASURE_REPRESENTATION_ITEM('density measure',
POSITIVE_RATIO_MEASURE(7850.),#8345);
#8393=MEASURE_REPRESENTATION_ITEM('density measure',
POSITIVE_RATIO_MEASURE(7850.),#8346);
#8394=MEASURE_REPRESENTATION_ITEM('density measure',
POSITIVE_RATIO_MEASURE(7850.),#8347);
#8395=MEASURE_REPRESENTATION_ITEM('density measure',
POSITIVE_RATIO_MEASURE(7850.),#8348);
#8396=MEASURE_REPRESENTATION_ITEM('density measure',
POSITIVE_RATIO_MEASURE(7850.),#8349);
#8397=MEASURE_REPRESENTATION_ITEM('density measure',
POSITIVE_RATIO_MEASURE(7850.),#8350);
#8398=MEASURE_REPRESENTATION_ITEM('density measure',
POSITIVE_RATIO_MEASURE(7850.),#8351);
#8399=MEASURE_REPRESENTATION_ITEM('density measure',
POSITIVE_RATIO_MEASURE(7850.),#8352);
#8400=MEASURE_REPRESENTATION_ITEM('density measure',
POSITIVE_RATIO_MEASURE(7850.),#8353);
#8401=MEASURE_REPRESENTATION_ITEM('density measure',
POSITIVE_RATIO_MEASURE(7850.),#8354);
#8402=MEASURE_REPRESENTATION_ITEM('density measure',
POSITIVE_RATIO_MEASURE(7850.),#8355);
#8403=MEASURE_REPRESENTATION_ITEM('density measure',
POSITIVE_RATIO_MEASURE(7850.),#8356);
#8404=MEASURE_REPRESENTATION_ITEM('density measure',
POSITIVE_RATIO_MEASURE(7850.),#8357);
#8405=MEASURE_REPRESENTATION_ITEM('density measure',
POSITIVE_RATIO_MEASURE(7850.),#8358);
#8406=MEASURE_REPRESENTATION_ITEM('density measure',
POSITIVE_RATIO_MEASURE(7850.),#8359);
#8407=MEASURE_REPRESENTATION_ITEM('density measure',
POSITIVE_RATIO_MEASURE(7850.),#8360);
#8408=MEASURE_REPRESENTATION_ITEM('density measure',
POSITIVE_RATIO_MEASURE(7850.),#8361);
#8409=MEASURE_REPRESENTATION_ITEM('density measure',
POSITIVE_RATIO_MEASURE(7850.),#8362);
#8410=MEASURE_REPRESENTATION_ITEM('density measure',
POSITIVE_RATIO_MEASURE(7850.),#8363);
#8411=MEASURE_REPRESENTATION_ITEM('density measure',
POSITIVE_RATIO_MEASURE(7850.),#8364);
#8412=MEASURE_REPRESENTATION_ITEM('density measure',
POSITIVE_RATIO_MEASURE(7850.),#8365);
#8413=PROPERTY_DEFINITION_REPRESENTATION(#8648,#8507);
#8414=PROPERTY_DEFINITION_REPRESENTATION(#8649,#8508);
#8415=PROPERTY_DEFINITION_REPRESENTATION(#8650,#8509);
#8416=PROPERTY_DEFINITION_REPRESENTATION(#8651,#8510);
#8417=PROPERTY_DEFINITION_REPRESENTATION(#8652,#8511);
#8418=PROPERTY_DEFINITION_REPRESENTATION(#8653,#8512);
#8419=PROPERTY_DEFINITION_REPRESENTATION(#8654,#8513);
#8420=PROPERTY_DEFINITION_REPRESENTATION(#8655,#8514);
#8421=PROPERTY_DEFINITION_REPRESENTATION(#8656,#8515);
#8422=PROPERTY_DEFINITION_REPRESENTATION(#8657,#8516);
#8423=PROPERTY_DEFINITION_REPRESENTATION(#8658,#8517);
#8424=PROPERTY_DEFINITION_REPRESENTATION(#8659,#8518);
#8425=PROPERTY_DEFINITION_REPRESENTATION(#8660,#8519);
#8426=PROPERTY_DEFINITION_REPRESENTATION(#8661,#8520);
#8427=PROPERTY_DEFINITION_REPRESENTATION(#8662,#8521);
#8428=PROPERTY_DEFINITION_REPRESENTATION(#8663,#8522);
#8429=PROPERTY_DEFINITION_REPRESENTATION(#8664,#8523);
#8430=PROPERTY_DEFINITION_REPRESENTATION(#8665,#8524);
#8431=PROPERTY_DEFINITION_REPRESENTATION(#8666,#8525);
#8432=PROPERTY_DEFINITION_REPRESENTATION(#8667,#8526);
#8433=PROPERTY_DEFINITION_REPRESENTATION(#8668,#8527);
#8434=PROPERTY_DEFINITION_REPRESENTATION(#8669,#8528);
#8435=PROPERTY_DEFINITION_REPRESENTATION(#8670,#8529);
#8436=PROPERTY_DEFINITION_REPRESENTATION(#8671,#8530);
#8437=PROPERTY_DEFINITION_REPRESENTATION(#8672,#8531);
#8438=PROPERTY_DEFINITION_REPRESENTATION(#8673,#8532);
#8439=PROPERTY_DEFINITION_REPRESENTATION(#8674,#8533);
#8440=PROPERTY_DEFINITION_REPRESENTATION(#8675,#8534);
#8441=PROPERTY_DEFINITION_REPRESENTATION(#8676,#8535);
#8442=PROPERTY_DEFINITION_REPRESENTATION(#8677,#8536);
#8443=PROPERTY_DEFINITION_REPRESENTATION(#8678,#8537);
#8444=PROPERTY_DEFINITION_REPRESENTATION(#8679,#8538);
#8445=PROPERTY_DEFINITION_REPRESENTATION(#8680,#8539);
#8446=PROPERTY_DEFINITION_REPRESENTATION(#8681,#8540);
#8447=PROPERTY_DEFINITION_REPRESENTATION(#8682,#8541);
#8448=PROPERTY_DEFINITION_REPRESENTATION(#8683,#8542);
#8449=PROPERTY_DEFINITION_REPRESENTATION(#8684,#8543);
#8450=PROPERTY_DEFINITION_REPRESENTATION(#8685,#8544);
#8451=PROPERTY_DEFINITION_REPRESENTATION(#8686,#8545);
#8452=PROPERTY_DEFINITION_REPRESENTATION(#8687,#8546);
#8453=PROPERTY_DEFINITION_REPRESENTATION(#8688,#8547);
#8454=PROPERTY_DEFINITION_REPRESENTATION(#8689,#8548);
#8455=PROPERTY_DEFINITION_REPRESENTATION(#8690,#8549);
#8456=PROPERTY_DEFINITION_REPRESENTATION(#8691,#8550);
#8457=PROPERTY_DEFINITION_REPRESENTATION(#8692,#8551);
#8458=PROPERTY_DEFINITION_REPRESENTATION(#8693,#8552);
#8459=PROPERTY_DEFINITION_REPRESENTATION(#8694,#8553);
#8460=PROPERTY_DEFINITION_REPRESENTATION(#8695,#8554);
#8461=PROPERTY_DEFINITION_REPRESENTATION(#8696,#8555);
#8462=PROPERTY_DEFINITION_REPRESENTATION(#8697,#8556);
#8463=PROPERTY_DEFINITION_REPRESENTATION(#8698,#8557);
#8464=PROPERTY_DEFINITION_REPRESENTATION(#8699,#8558);
#8465=PROPERTY_DEFINITION_REPRESENTATION(#8700,#8559);
#8466=PROPERTY_DEFINITION_REPRESENTATION(#8701,#8560);
#8467=PROPERTY_DEFINITION_REPRESENTATION(#8702,#8561);
#8468=PROPERTY_DEFINITION_REPRESENTATION(#8703,#8562);
#8469=PROPERTY_DEFINITION_REPRESENTATION(#8704,#8563);
#8470=PROPERTY_DEFINITION_REPRESENTATION(#8705,#8564);
#8471=PROPERTY_DEFINITION_REPRESENTATION(#8706,#8565);
#8472=PROPERTY_DEFINITION_REPRESENTATION(#8707,#8566);
#8473=PROPERTY_DEFINITION_REPRESENTATION(#8708,#8567);
#8474=PROPERTY_DEFINITION_REPRESENTATION(#8709,#8568);
#8475=PROPERTY_DEFINITION_REPRESENTATION(#8710,#8569);
#8476=PROPERTY_DEFINITION_REPRESENTATION(#8711,#8570);
#8477=PROPERTY_DEFINITION_REPRESENTATION(#8712,#8571);
#8478=PROPERTY_DEFINITION_REPRESENTATION(#8713,#8572);
#8479=PROPERTY_DEFINITION_REPRESENTATION(#8714,#8573);
#8480=PROPERTY_DEFINITION_REPRESENTATION(#8715,#8574);
#8481=PROPERTY_DEFINITION_REPRESENTATION(#8716,#8575);
#8482=PROPERTY_DEFINITION_REPRESENTATION(#8717,#8576);
#8483=PROPERTY_DEFINITION_REPRESENTATION(#8718,#8577);
#8484=PROPERTY_DEFINITION_REPRESENTATION(#8719,#8578);
#8485=PROPERTY_DEFINITION_REPRESENTATION(#8720,#8579);
#8486=PROPERTY_DEFINITION_REPRESENTATION(#8721,#8580);
#8487=PROPERTY_DEFINITION_REPRESENTATION(#8722,#8581);
#8488=PROPERTY_DEFINITION_REPRESENTATION(#8723,#8582);
#8489=PROPERTY_DEFINITION_REPRESENTATION(#8724,#8583);
#8490=PROPERTY_DEFINITION_REPRESENTATION(#8725,#8584);
#8491=PROPERTY_DEFINITION_REPRESENTATION(#8726,#8585);
#8492=PROPERTY_DEFINITION_REPRESENTATION(#8727,#8586);
#8493=PROPERTY_DEFINITION_REPRESENTATION(#8728,#8587);
#8494=PROPERTY_DEFINITION_REPRESENTATION(#8729,#8588);
#8495=PROPERTY_DEFINITION_REPRESENTATION(#8730,#8589);
#8496=PROPERTY_DEFINITION_REPRESENTATION(#8731,#8590);
#8497=PROPERTY_DEFINITION_REPRESENTATION(#8732,#8591);
#8498=PROPERTY_DEFINITION_REPRESENTATION(#8733,#8592);
#8499=PROPERTY_DEFINITION_REPRESENTATION(#8734,#8593);
#8500=PROPERTY_DEFINITION_REPRESENTATION(#8735,#8594);
#8501=PROPERTY_DEFINITION_REPRESENTATION(#8736,#8595);
#8502=PROPERTY_DEFINITION_REPRESENTATION(#8737,#8596);
#8503=PROPERTY_DEFINITION_REPRESENTATION(#8738,#8597);
#8504=PROPERTY_DEFINITION_REPRESENTATION(#8739,#8598);
#8505=PROPERTY_DEFINITION_REPRESENTATION(#8740,#8599);
#8506=PROPERTY_DEFINITION_REPRESENTATION(#8741,#8600);
#8507=REPRESENTATION('material name',(#8601),#16996);
#8508=REPRESENTATION('density',(#8366),#16996);
#8509=REPRESENTATION('material name',(#8602),#16997);
#8510=REPRESENTATION('density',(#8367),#16997);
#8511=REPRESENTATION('material name',(#8603),#16998);
#8512=REPRESENTATION('density',(#8368),#16998);
#8513=REPRESENTATION('material name',(#8604),#16999);
#8514=REPRESENTATION('density',(#8369),#16999);
#8515=REPRESENTATION('material name',(#8605),#17000);
#8516=REPRESENTATION('density',(#8370),#17000);
#8517=REPRESENTATION('material name',(#8606),#17001);
#8518=REPRESENTATION('density',(#8371),#17001);
#8519=REPRESENTATION('material name',(#8607),#17002);
#8520=REPRESENTATION('density',(#8372),#17002);
#8521=REPRESENTATION('material name',(#8608),#17003);
#8522=REPRESENTATION('density',(#8373),#17003);
#8523=REPRESENTATION('material name',(#8609),#17004);
#8524=REPRESENTATION('density',(#8374),#17004);
#8525=REPRESENTATION('material name',(#8610),#17005);
#8526=REPRESENTATION('density',(#8375),#17005);
#8527=REPRESENTATION('material name',(#8611),#17006);
#8528=REPRESENTATION('density',(#8376),#17006);
#8529=REPRESENTATION('material name',(#8612),#17007);
#8530=REPRESENTATION('density',(#8377),#17007);
#8531=REPRESENTATION('material name',(#8613),#17008);
#8532=REPRESENTATION('density',(#8378),#17008);
#8533=REPRESENTATION('material name',(#8614),#17009);
#8534=REPRESENTATION('density',(#8379),#17009);
#8535=REPRESENTATION('material name',(#8615),#17010);
#8536=REPRESENTATION('density',(#8380),#17010);
#8537=REPRESENTATION('material name',(#8616),#17011);
#8538=REPRESENTATION('density',(#8381),#17011);
#8539=REPRESENTATION('material name',(#8617),#17012);
#8540=REPRESENTATION('density',(#8382),#17012);
#8541=REPRESENTATION('material name',(#8618),#17013);
#8542=REPRESENTATION('density',(#8383),#17013);
#8543=REPRESENTATION('material name',(#8619),#17014);
#8544=REPRESENTATION('density',(#8384),#17014);
#8545=REPRESENTATION('material name',(#8620),#17015);
#8546=REPRESENTATION('density',(#8385),#17015);
#8547=REPRESENTATION('material name',(#8621),#17016);
#8548=REPRESENTATION('density',(#8386),#17016);
#8549=REPRESENTATION('material name',(#8622),#17017);
#8550=REPRESENTATION('density',(#8387),#17017);
#8551=REPRESENTATION('material name',(#8623),#17018);
#8552=REPRESENTATION('density',(#8388),#17018);
#8553=REPRESENTATION('material name',(#8624),#17019);
#8554=REPRESENTATION('density',(#8389),#17019);
#8555=REPRESENTATION('material name',(#8625),#17021);
#8556=REPRESENTATION('density',(#8390),#17021);
#8557=REPRESENTATION('material name',(#8626),#17022);
#8558=REPRESENTATION('density',(#8391),#17022);
#8559=REPRESENTATION('material name',(#8627),#17023);
#8560=REPRESENTATION('density',(#8392),#17023);
#8561=REPRESENTATION('material name',(#8628),#17024);
#8562=REPRESENTATION('density',(#8393),#17024);
#8563=REPRESENTATION('material name',(#8629),#17025);
#8564=REPRESENTATION('density',(#8394),#17025);
#8565=REPRESENTATION('material name',(#8630),#17026);
#8566=REPRESENTATION('density',(#8395),#17026);
#8567=REPRESENTATION('material name',(#8631),#17027);
#8568=REPRESENTATION('density',(#8396),#17027);
#8569=REPRESENTATION('material name',(#8632),#17028);
#8570=REPRESENTATION('density',(#8397),#17028);
#8571=REPRESENTATION('material name',(#8633),#17030);
#8572=REPRESENTATION('density',(#8398),#17030);
#8573=REPRESENTATION('material name',(#8634),#17031);
#8574=REPRESENTATION('density',(#8399),#17031);
#8575=REPRESENTATION('material name',(#8635),#17032);
#8576=REPRESENTATION('density',(#8400),#17032);
#8577=REPRESENTATION('material name',(#8636),#17033);
#8578=REPRESENTATION('density',(#8401),#17033);
#8579=REPRESENTATION('material name',(#8637),#17034);
#8580=REPRESENTATION('density',(#8402),#17034);
#8581=REPRESENTATION('material name',(#8638),#17035);
#8582=REPRESENTATION('density',(#8403),#17035);
#8583=REPRESENTATION('material name',(#8639),#17036);
#8584=REPRESENTATION('density',(#8404),#17036);
#8585=REPRESENTATION('material name',(#8640),#17038);
#8586=REPRESENTATION('density',(#8405),#17038);
#8587=REPRESENTATION('material name',(#8641),#17039);
#8588=REPRESENTATION('density',(#8406),#17039);
#8589=REPRESENTATION('material name',(#8642),#17040);
#8590=REPRESENTATION('density',(#8407),#17040);
#8591=REPRESENTATION('material name',(#8643),#17041);
#8592=REPRESENTATION('density',(#8408),#17041);
#8593=REPRESENTATION('material name',(#8644),#17042);
#8594=REPRESENTATION('density',(#8409),#17042);
#8595=REPRESENTATION('material name',(#8645),#17043);
#8596=REPRESENTATION('density',(#8410),#17043);
#8597=REPRESENTATION('material name',(#8646),#17044);
#8598=REPRESENTATION('density',(#8411),#17044);
#8599=REPRESENTATION('material name',(#8647),#17045);
#8600=REPRESENTATION('density',(#8412),#17045);
#8601=DESCRIPTIVE_REPRESENTATION_ITEM('Steel','Steel');
#8602=DESCRIPTIVE_REPRESENTATION_ITEM('Steel','Steel');
#8603=DESCRIPTIVE_REPRESENTATION_ITEM('Steel','Steel');
#8604=DESCRIPTIVE_REPRESENTATION_ITEM('Steel','Steel');
#8605=DESCRIPTIVE_REPRESENTATION_ITEM('Steel','Steel');
#8606=DESCRIPTIVE_REPRESENTATION_ITEM('Steel','Steel');
#8607=DESCRIPTIVE_REPRESENTATION_ITEM('Steel','Steel');
#8608=DESCRIPTIVE_REPRESENTATION_ITEM('Steel','Steel');
#8609=DESCRIPTIVE_REPRESENTATION_ITEM('Steel','Steel');
#8610=DESCRIPTIVE_REPRESENTATION_ITEM('Steel','Steel');
#8611=DESCRIPTIVE_REPRESENTATION_ITEM('Steel','Steel');
#8612=DESCRIPTIVE_REPRESENTATION_ITEM('Steel','Steel');
#8613=DESCRIPTIVE_REPRESENTATION_ITEM('Steel','Steel');
#8614=DESCRIPTIVE_REPRESENTATION_ITEM('Steel','Steel');
#8615=DESCRIPTIVE_REPRESENTATION_ITEM('Steel','Steel');
#8616=DESCRIPTIVE_REPRESENTATION_ITEM('Steel','Steel');
#8617=DESCRIPTIVE_REPRESENTATION_ITEM('Steel','Steel');
#8618=DESCRIPTIVE_REPRESENTATION_ITEM('Steel','Steel');
#8619=DESCRIPTIVE_REPRESENTATION_ITEM('Steel','Steel');
#8620=DESCRIPTIVE_REPRESENTATION_ITEM('Steel','Steel');
#8621=DESCRIPTIVE_REPRESENTATION_ITEM('Steel','Steel');
#8622=DESCRIPTIVE_REPRESENTATION_ITEM('Steel','Steel');
#8623=DESCRIPTIVE_REPRESENTATION_ITEM('Steel','Steel');
#8624=DESCRIPTIVE_REPRESENTATION_ITEM('Steel','Steel');
#8625=DESCRIPTIVE_REPRESENTATION_ITEM('Steel','Steel');
#8626=DESCRIPTIVE_REPRESENTATION_ITEM('Steel','Steel');
#8627=DESCRIPTIVE_REPRESENTATION_ITEM('Steel','Steel');
#8628=DESCRIPTIVE_REPRESENTATION_ITEM('Steel','Steel');
#8629=DESCRIPTIVE_REPRESENTATION_ITEM('Steel','Steel');
#8630=DESCRIPTIVE_REPRESENTATION_ITEM('Steel','Steel');
#8631=DESCRIPTIVE_REPRESENTATION_ITEM('Steel','Steel');
#8632=DESCRIPTIVE_REPRESENTATION_ITEM('Steel','Steel');
#8633=DESCRIPTIVE_REPRESENTATION_ITEM('Steel','Steel');
#8634=DESCRIPTIVE_REPRESENTATION_ITEM('Steel','Steel');
#8635=DESCRIPTIVE_REPRESENTATION_ITEM('Steel','Steel');
#8636=DESCRIPTIVE_REPRESENTATION_ITEM('Steel','Steel');
#8637=DESCRIPTIVE_REPRESENTATION_ITEM('Steel','Steel');
#8638=DESCRIPTIVE_REPRESENTATION_ITEM('Steel','Steel');
#8639=DESCRIPTIVE_REPRESENTATION_ITEM('Steel','Steel');
#8640=DESCRIPTIVE_REPRESENTATION_ITEM('Steel','Steel');
#8641=DESCRIPTIVE_REPRESENTATION_ITEM('Steel','Steel');
#8642=DESCRIPTIVE_REPRESENTATION_ITEM('Steel','Steel');
#8643=DESCRIPTIVE_REPRESENTATION_ITEM('Steel','Steel');
#8644=DESCRIPTIVE_REPRESENTATION_ITEM('Steel','Steel');
#8645=DESCRIPTIVE_REPRESENTATION_ITEM('Steel','Steel');
#8646=DESCRIPTIVE_REPRESENTATION_ITEM('Steel','Steel');
#8647=DESCRIPTIVE_REPRESENTATION_ITEM('Steel','Steel');
#8648=PROPERTY_DEFINITION('material property','material name',#17313);
#8649=PROPERTY_DEFINITION('material property','density of part',#17313);
#8650=PROPERTY_DEFINITION('material property','material name',#17314);
#8651=PROPERTY_DEFINITION('material property','density of part',#17314);
#8652=PROPERTY_DEFINITION('material property','material name',#17315);
#8653=PROPERTY_DEFINITION('material property','density of part',#17315);
#8654=PROPERTY_DEFINITION('material property','material name',#17316);
#8655=PROPERTY_DEFINITION('material property','density of part',#17316);
#8656=PROPERTY_DEFINITION('material property','material name',#17317);
#8657=PROPERTY_DEFINITION('material property','density of part',#17317);
#8658=PROPERTY_DEFINITION('material property','material name',#17318);
#8659=PROPERTY_DEFINITION('material property','density of part',#17318);
#8660=PROPERTY_DEFINITION('material property','material name',#17319);
#8661=PROPERTY_DEFINITION('material property','density of part',#17319);
#8662=PROPERTY_DEFINITION('material property','material name',#17320);
#8663=PROPERTY_DEFINITION('material property','density of part',#17320);
#8664=PROPERTY_DEFINITION('material property','material name',#17321);
#8665=PROPERTY_DEFINITION('material property','density of part',#17321);
#8666=PROPERTY_DEFINITION('material property','material name',#17322);
#8667=PROPERTY_DEFINITION('material property','density of part',#17322);
#8668=PROPERTY_DEFINITION('material property','material name',#17323);
#8669=PROPERTY_DEFINITION('material property','density of part',#17323);
#8670=PROPERTY_DEFINITION('material property','material name',#17324);
#8671=PROPERTY_DEFINITION('material property','density of part',#17324);
#8672=PROPERTY_DEFINITION('material property','material name',#17325);
#8673=PROPERTY_DEFINITION('material property','density of part',#17325);
#8674=PROPERTY_DEFINITION('material property','material name',#17326);
#8675=PROPERTY_DEFINITION('material property','density of part',#17326);
#8676=PROPERTY_DEFINITION('material property','material name',#17327);
#8677=PROPERTY_DEFINITION('material property','density of part',#17327);
#8678=PROPERTY_DEFINITION('material property','material name',#17328);
#8679=PROPERTY_DEFINITION('material property','density of part',#17328);
#8680=PROPERTY_DEFINITION('material property','material name',#17329);
#8681=PROPERTY_DEFINITION('material property','density of part',#17329);
#8682=PROPERTY_DEFINITION('material property','material name',#17330);
#8683=PROPERTY_DEFINITION('material property','density of part',#17330);
#8684=PROPERTY_DEFINITION('material property','material name',#17331);
#8685=PROPERTY_DEFINITION('material property','density of part',#17331);
#8686=PROPERTY_DEFINITION('material property','material name',#17332);
#8687=PROPERTY_DEFINITION('material property','density of part',#17332);
#8688=PROPERTY_DEFINITION('material property','material name',#17333);
#8689=PROPERTY_DEFINITION('material property','density of part',#17333);
#8690=PROPERTY_DEFINITION('material property','material name',#17334);
#8691=PROPERTY_DEFINITION('material property','density of part',#17334);
#8692=PROPERTY_DEFINITION('material property','material name',#17335);
#8693=PROPERTY_DEFINITION('material property','density of part',#17335);
#8694=PROPERTY_DEFINITION('material property','material name',#17336);
#8695=PROPERTY_DEFINITION('material property','density of part',#17336);
#8696=PROPERTY_DEFINITION('material property','material name',#17338);
#8697=PROPERTY_DEFINITION('material property','density of part',#17338);
#8698=PROPERTY_DEFINITION('material property','material name',#17339);
#8699=PROPERTY_DEFINITION('material property','density of part',#17339);
#8700=PROPERTY_DEFINITION('material property','material name',#17340);
#8701=PROPERTY_DEFINITION('material property','density of part',#17340);
#8702=PROPERTY_DEFINITION('material property','material name',#17341);
#8703=PROPERTY_DEFINITION('material property','density of part',#17341);
#8704=PROPERTY_DEFINITION('material property','material name',#17342);
#8705=PROPERTY_DEFINITION('material property','density of part',#17342);
#8706=PROPERTY_DEFINITION('material property','material name',#17343);
#8707=PROPERTY_DEFINITION('material property','density of part',#17343);
#8708=PROPERTY_DEFINITION('material property','material name',#17344);
#8709=PROPERTY_DEFINITION('material property','density of part',#17344);
#8710=PROPERTY_DEFINITION('material property','material name',#17345);
#8711=PROPERTY_DEFINITION('material property','density of part',#17345);
#8712=PROPERTY_DEFINITION('material property','material name',#17347);
#8713=PROPERTY_DEFINITION('material property','density of part',#17347);
#8714=PROPERTY_DEFINITION('material property','material name',#17348);
#8715=PROPERTY_DEFINITION('material property','density of part',#17348);
#8716=PROPERTY_DEFINITION('material property','material name',#17349);
#8717=PROPERTY_DEFINITION('material property','density of part',#17349);
#8718=PROPERTY_DEFINITION('material property','material name',#17350);
#8719=PROPERTY_DEFINITION('material property','density of part',#17350);
#8720=PROPERTY_DEFINITION('material property','material name',#17351);
#8721=PROPERTY_DEFINITION('material property','density of part',#17351);
#8722=PROPERTY_DEFINITION('material property','material name',#17352);
#8723=PROPERTY_DEFINITION('material property','density of part',#17352);
#8724=PROPERTY_DEFINITION('material property','material name',#17353);
#8725=PROPERTY_DEFINITION('material property','density of part',#17353);
#8726=PROPERTY_DEFINITION('material property','material name',#17355);
#8727=PROPERTY_DEFINITION('material property','density of part',#17355);
#8728=PROPERTY_DEFINITION('material property','material name',#17356);
#8729=PROPERTY_DEFINITION('material property','density of part',#17356);
#8730=PROPERTY_DEFINITION('material property','material name',#17357);
#8731=PROPERTY_DEFINITION('material property','density of part',#17357);
#8732=PROPERTY_DEFINITION('material property','material name',#17358);
#8733=PROPERTY_DEFINITION('material property','density of part',#17358);
#8734=PROPERTY_DEFINITION('material property','material name',#17359);
#8735=PROPERTY_DEFINITION('material property','density of part',#17359);
#8736=PROPERTY_DEFINITION('material property','material name',#17360);
#8737=PROPERTY_DEFINITION('material property','density of part',#17360);
#8738=PROPERTY_DEFINITION('material property','material name',#17361);
#8739=PROPERTY_DEFINITION('material property','density of part',#17361);
#8740=PROPERTY_DEFINITION('material property','material name',#17362);
#8741=PROPERTY_DEFINITION('material property','density of part',#17362);
#8742=AXIS2_PLACEMENT_3D('',#12375,#9773,#9774);
#8743=AXIS2_PLACEMENT_3D('',#12376,#9775,#9776);
#8744=AXIS2_PLACEMENT_3D('',#12377,#9777,#9778);
#8745=AXIS2_PLACEMENT_3D('',#12378,#9779,#9780);
#8746=AXIS2_PLACEMENT_3D('',#12380,#9781,#9782);
#8747=AXIS2_PLACEMENT_3D('',#12383,#9784,#9785);
#8748=AXIS2_PLACEMENT_3D('',#12384,#9786,#9787);
#8749=AXIS2_PLACEMENT_3D('',#12386,#9788,#9789);
#8750=AXIS2_PLACEMENT_3D('',#12389,#9791,#9792);
#8751=AXIS2_PLACEMENT_3D('',#12390,#9793,#9794);
#8752=AXIS2_PLACEMENT_3D('',#12392,#9795,#9796);
#8753=AXIS2_PLACEMENT_3D('',#12395,#9798,#9799);
#8754=AXIS2_PLACEMENT_3D('',#12396,#9800,#9801);
#8755=AXIS2_PLACEMENT_3D('',#12398,#9802,#9803);
#8756=AXIS2_PLACEMENT_3D('',#12401,#9805,#9806);
#8757=AXIS2_PLACEMENT_3D('',#12402,#9807,#9808);
#8758=AXIS2_PLACEMENT_3D('',#12404,#9809,#9810);
#8759=AXIS2_PLACEMENT_3D('',#12407,#9812,#9813);
#8760=AXIS2_PLACEMENT_3D('',#12408,#9814,#9815);
#8761=AXIS2_PLACEMENT_3D('',#12410,#9816,#9817);
#8762=AXIS2_PLACEMENT_3D('',#12413,#9819,#9820);
#8763=AXIS2_PLACEMENT_3D('',#12414,#9821,#9822);
#8764=AXIS2_PLACEMENT_3D('',#12416,#9823,#9824);
#8765=AXIS2_PLACEMENT_3D('',#12419,#9826,#9827);
#8766=AXIS2_PLACEMENT_3D('',#12420,#9828,#9829);
#8767=AXIS2_PLACEMENT_3D('',#12422,#9830,#9831);
#8768=AXIS2_PLACEMENT_3D('',#12425,#9833,#9834);
#8769=AXIS2_PLACEMENT_3D('',#12426,#9835,#9836);
#8770=AXIS2_PLACEMENT_3D('',#12428,#9837,#9838);
#8771=AXIS2_PLACEMENT_3D('',#12431,#9840,#9841);
#8772=AXIS2_PLACEMENT_3D('',#12432,#9842,#9843);
#8773=AXIS2_PLACEMENT_3D('',#12434,#9844,#9845);
#8774=AXIS2_PLACEMENT_3D('',#12437,#9847,#9848);
#8775=AXIS2_PLACEMENT_3D('',#12438,#9849,#9850);
#8776=AXIS2_PLACEMENT_3D('',#12447,#9855,#9856);
#8777=AXIS2_PLACEMENT_3D('',#12453,#9860,#9861);
#8778=AXIS2_PLACEMENT_3D('',#12459,#9865,#9866);
#8779=AXIS2_PLACEMENT_3D('',#12462,#9869,#9870);
#8780=AXIS2_PLACEMENT_3D('',#12463,#9871,#9872);
#8781=AXIS2_PLACEMENT_3D('',#12464,#9873,#9874);
#8782=AXIS2_PLACEMENT_3D('',#12465,#9875,#9876);
#8783=AXIS2_PLACEMENT_3D('',#12474,#9881,#9882);
#8784=AXIS2_PLACEMENT_3D('',#12480,#9886,#9887);
#8785=AXIS2_PLACEMENT_3D('',#12486,#9891,#9892);
#8786=AXIS2_PLACEMENT_3D('',#12489,#9895,#9896);
#8787=AXIS2_PLACEMENT_3D('',#12490,#9897,#9898);
#8788=AXIS2_PLACEMENT_3D('',#12491,#9899,#9900);
#8789=AXIS2_PLACEMENT_3D('',#12492,#9901,#9902);
#8790=AXIS2_PLACEMENT_3D('',#12501,#9907,#9908);
#8791=AXIS2_PLACEMENT_3D('',#12507,#9912,#9913);
#8792=AXIS2_PLACEMENT_3D('',#12513,#9917,#9918);
#8793=AXIS2_PLACEMENT_3D('',#12516,#9921,#9922);
#8794=AXIS2_PLACEMENT_3D('',#12517,#9923,#9924);
#8795=AXIS2_PLACEMENT_3D('',#12518,#9925,#9926);
#8796=AXIS2_PLACEMENT_3D('',#12519,#9927,#9928);
#8797=AXIS2_PLACEMENT_3D('',#12521,#9929,#9930);
#8798=AXIS2_PLACEMENT_3D('',#12524,#9932,#9933);
#8799=AXIS2_PLACEMENT_3D('',#12525,#9934,#9935);
#8800=AXIS2_PLACEMENT_3D('',#12527,#9936,#9937);
#8801=AXIS2_PLACEMENT_3D('',#12530,#9939,#9940);
#8802=AXIS2_PLACEMENT_3D('',#12531,#9941,#9942);
#8803=AXIS2_PLACEMENT_3D('',#12533,#9943,#9944);
#8804=AXIS2_PLACEMENT_3D('',#12536,#9946,#9947);
#8805=AXIS2_PLACEMENT_3D('',#12537,#9948,#9949);
#8806=AXIS2_PLACEMENT_3D('',#12539,#9950,#9951);
#8807=AXIS2_PLACEMENT_3D('',#12542,#9953,#9954);
#8808=AXIS2_PLACEMENT_3D('',#12543,#9955,#9956);
#8809=AXIS2_PLACEMENT_3D('',#12548,#9958,#9959);
#8810=AXIS2_PLACEMENT_3D('',#12551,#9961,#9962);
#8811=AXIS2_PLACEMENT_3D('',#12552,#9963,#9964);
#8812=AXIS2_PLACEMENT_3D('',#12557,#9966,#9967);
#8813=AXIS2_PLACEMENT_3D('',#12560,#9969,#9970);
#8814=AXIS2_PLACEMENT_3D('',#12561,#9971,#9972);
#8815=AXIS2_PLACEMENT_3D('',#12574,#9979,#9980);
#8816=AXIS2_PLACEMENT_3D('',#12578,#9982,#9983);
#8817=AXIS2_PLACEMENT_3D('',#12582,#9985,#9986);
#8818=AXIS2_PLACEMENT_3D('',#12586,#9988,#9989);
#8819=AXIS2_PLACEMENT_3D('',#12590,#9991,#9992);
#8820=AXIS2_PLACEMENT_3D('',#12594,#9994,#9995);
#8821=AXIS2_PLACEMENT_3D('',#12596,#9997,#9998);
#8822=AXIS2_PLACEMENT_3D('',#12598,#10000,#10001);
#8823=AXIS2_PLACEMENT_3D('',#12600,#10003,#10004);
#8824=AXIS2_PLACEMENT_3D('',#12605,#10007,#10008);
#8825=AXIS2_PLACEMENT_3D('',#12606,#10009,#10010);
#8826=AXIS2_PLACEMENT_3D('',#12611,#10013,#10014);
#8827=AXIS2_PLACEMENT_3D('',#12612,#10015,#10016);
#8828=AXIS2_PLACEMENT_3D('',#12614,#10018,#10019);
#8829=AXIS2_PLACEMENT_3D('',#12616,#10021,#10022);
#8830=AXIS2_PLACEMENT_3D('',#12621,#10025,#10026);
#8831=AXIS2_PLACEMENT_3D('',#12622,#10027,#10028);
#8832=AXIS2_PLACEMENT_3D('',#12627,#10031,#10032);
#8833=AXIS2_PLACEMENT_3D('',#12628,#10033,#10034);
#8834=AXIS2_PLACEMENT_3D('',#12630,#10036,#10037);
#8835=AXIS2_PLACEMENT_3D('',#12632,#10039,#10040);
#8836=AXIS2_PLACEMENT_3D('',#12637,#10043,#10044);
#8837=AXIS2_PLACEMENT_3D('',#12638,#10045,#10046);
#8838=AXIS2_PLACEMENT_3D('',#12643,#10049,#10050);
#8839=AXIS2_PLACEMENT_3D('',#12644,#10051,#10052);
#8840=AXIS2_PLACEMENT_3D('',#12646,#10054,#10055);
#8841=AXIS2_PLACEMENT_3D('',#12648,#10057,#10058);
#8842=AXIS2_PLACEMENT_3D('',#12654,#10062,#10063);
#8843=AXIS2_PLACEMENT_3D('',#12658,#10066,#10067);
#8844=AXIS2_PLACEMENT_3D('',#12662,#10070,#10071);
#8845=AXIS2_PLACEMENT_3D('',#12664,#10073,#10074);
#8846=AXIS2_PLACEMENT_3D('',#12665,#10075,#10076);
#8847=AXIS2_PLACEMENT_3D('',#12666,#10077,#10078);
#8848=AXIS2_PLACEMENT_3D('',#12668,#10079,#10080);
#8849=AXIS2_PLACEMENT_3D('',#12671,#10082,#10083);
#8850=AXIS2_PLACEMENT_3D('',#12672,#10084,#10085);
#8851=AXIS2_PLACEMENT_3D('',#12674,#10086,#10087);
#8852=AXIS2_PLACEMENT_3D('',#12677,#10089,#10090);
#8853=AXIS2_PLACEMENT_3D('',#12678,#10091,#10092);
#8854=AXIS2_PLACEMENT_3D('',#12680,#10093,#10094);
#8855=AXIS2_PLACEMENT_3D('',#12683,#10096,#10097);
#8856=AXIS2_PLACEMENT_3D('',#12684,#10098,#10099);
#8857=AXIS2_PLACEMENT_3D('',#12686,#10100,#10101);
#8858=AXIS2_PLACEMENT_3D('',#12689,#10103,#10104);
#8859=AXIS2_PLACEMENT_3D('',#12690,#10105,#10106);
#8860=AXIS2_PLACEMENT_3D('',#12692,#10107,#10108);
#8861=AXIS2_PLACEMENT_3D('',#12695,#10110,#10111);
#8862=AXIS2_PLACEMENT_3D('',#12696,#10112,#10113);
#8863=AXIS2_PLACEMENT_3D('',#12698,#10114,#10115);
#8864=AXIS2_PLACEMENT_3D('',#12701,#10117,#10118);
#8865=AXIS2_PLACEMENT_3D('',#12702,#10119,#10120);
#8866=AXIS2_PLACEMENT_3D('',#12704,#10121,#10122);
#8867=AXIS2_PLACEMENT_3D('',#12707,#10124,#10125);
#8868=AXIS2_PLACEMENT_3D('',#12708,#10126,#10127);
#8869=AXIS2_PLACEMENT_3D('',#12717,#10132,#10133);
#8870=AXIS2_PLACEMENT_3D('',#12726,#10138,#10139);
#8871=AXIS2_PLACEMENT_3D('',#12732,#10143,#10144);
#8872=AXIS2_PLACEMENT_3D('',#12738,#10148,#10149);
#8873=AXIS2_PLACEMENT_3D('',#12745,#10154,#10155);
#8874=AXIS2_PLACEMENT_3D('',#12749,#10158,#10159);
#8875=AXIS2_PLACEMENT_3D('',#12754,#10163,#10164);
#8876=AXIS2_PLACEMENT_3D('',#12756,#10166,#10167);
#8877=AXIS2_PLACEMENT_3D('',#12757,#10168,#10169);
#8878=AXIS2_PLACEMENT_3D('',#12758,#10170,#10171);
#8879=AXIS2_PLACEMENT_3D('',#12759,#10172,#10173);
#8880=AXIS2_PLACEMENT_3D('',#12761,#10174,#10175);
#8881=AXIS2_PLACEMENT_3D('',#12764,#10177,#10178);
#8882=AXIS2_PLACEMENT_3D('',#12765,#10179,#10180);
#8883=AXIS2_PLACEMENT_3D('',#12767,#10181,#10182);
#8884=AXIS2_PLACEMENT_3D('',#12770,#10184,#10185);
#8885=AXIS2_PLACEMENT_3D('',#12771,#10186,#10187);
#8886=AXIS2_PLACEMENT_3D('',#12773,#10188,#10189);
#8887=AXIS2_PLACEMENT_3D('',#12776,#10191,#10192);
#8888=AXIS2_PLACEMENT_3D('',#12777,#10193,#10194);
#8889=AXIS2_PLACEMENT_3D('',#12779,#10195,#10196);
#8890=AXIS2_PLACEMENT_3D('',#12782,#10198,#10199);
#8891=AXIS2_PLACEMENT_3D('',#12783,#10200,#10201);
#8892=AXIS2_PLACEMENT_3D('',#12785,#10202,#10203);
#8893=AXIS2_PLACEMENT_3D('',#12788,#10205,#10206);
#8894=AXIS2_PLACEMENT_3D('',#12789,#10207,#10208);
#8895=AXIS2_PLACEMENT_3D('',#12791,#10209,#10210);
#8896=AXIS2_PLACEMENT_3D('',#12792,#10211,#10212);
#8897=AXIS2_PLACEMENT_3D('',#12795,#10214,#10215);
#8898=AXIS2_PLACEMENT_3D('',#12796,#10216,#10217);
#8899=AXIS2_PLACEMENT_3D('',#12798,#10218,#10219);
#8900=AXIS2_PLACEMENT_3D('',#12801,#10221,#10222);
#8901=AXIS2_PLACEMENT_3D('',#12802,#10223,#10224);
#8902=AXIS2_PLACEMENT_3D('',#12803,#10225,#10226);
#8903=AXIS2_PLACEMENT_3D('',#12804,#10227,#10228);
#8904=AXIS2_PLACEMENT_3D('',#12805,#10229,#10230);
#8905=AXIS2_PLACEMENT_3D('',#12807,#10231,#10232);
#8906=AXIS2_PLACEMENT_3D('',#12810,#10234,#10235);
#8907=AXIS2_PLACEMENT_3D('',#12811,#10236,#10237);
#8908=AXIS2_PLACEMENT_3D('',#12813,#10238,#10239);
#8909=AXIS2_PLACEMENT_3D('',#12816,#10241,#10242);
#8910=AXIS2_PLACEMENT_3D('',#12817,#10243,#10244);
#8911=AXIS2_PLACEMENT_3D('',#12819,#10245,#10246);
#8912=AXIS2_PLACEMENT_3D('',#12822,#10248,#10249);
#8913=AXIS2_PLACEMENT_3D('',#12823,#10250,#10251);
#8914=AXIS2_PLACEMENT_3D('',#12825,#10252,#10253);
#8915=AXIS2_PLACEMENT_3D('',#12828,#10255,#10256);
#8916=AXIS2_PLACEMENT_3D('',#12829,#10257,#10258);
#8917=AXIS2_PLACEMENT_3D('',#12831,#10259,#10260);
#8918=AXIS2_PLACEMENT_3D('',#12834,#10262,#10263);
#8919=AXIS2_PLACEMENT_3D('',#12835,#10264,#10265);
#8920=AXIS2_PLACEMENT_3D('',#12837,#10266,#10267);
#8921=AXIS2_PLACEMENT_3D('',#12838,#10268,#10269);
#8922=AXIS2_PLACEMENT_3D('',#12840,#10270,#10271);
#8923=AXIS2_PLACEMENT_3D('',#12842,#10273,#10274);
#8924=AXIS2_PLACEMENT_3D('',#12844,#10275,#10276);
#8925=AXIS2_PLACEMENT_3D('',#12847,#10278,#10279);
#8926=AXIS2_PLACEMENT_3D('',#12848,#10280,#10281);
#8927=AXIS2_PLACEMENT_3D('',#12849,#10282,#10283);
#8928=AXIS2_PLACEMENT_3D('',#12850,#10284,#10285);
#8929=AXIS2_PLACEMENT_3D('',#12851,#10286,#10287);
#8930=AXIS2_PLACEMENT_3D('',#12853,#10288,#10289);
#8931=AXIS2_PLACEMENT_3D('',#12856,#10291,#10292);
#8932=AXIS2_PLACEMENT_3D('',#12857,#10293,#10294);
#8933=AXIS2_PLACEMENT_3D('',#12859,#10295,#10296);
#8934=AXIS2_PLACEMENT_3D('',#12862,#10298,#10299);
#8935=AXIS2_PLACEMENT_3D('',#12863,#10300,#10301);
#8936=AXIS2_PLACEMENT_3D('',#12865,#10302,#10303);
#8937=AXIS2_PLACEMENT_3D('',#12868,#10305,#10306);
#8938=AXIS2_PLACEMENT_3D('',#12869,#10307,#10308);
#8939=AXIS2_PLACEMENT_3D('',#12871,#10309,#10310);
#8940=AXIS2_PLACEMENT_3D('',#12874,#10312,#10313);
#8941=AXIS2_PLACEMENT_3D('',#12875,#10314,#10315);
#8942=AXIS2_PLACEMENT_3D('',#12877,#10316,#10317);
#8943=AXIS2_PLACEMENT_3D('',#12880,#10319,#10320);
#8944=AXIS2_PLACEMENT_3D('',#12881,#10321,#10322);
#8945=AXIS2_PLACEMENT_3D('',#12883,#10323,#10324);
#8946=AXIS2_PLACEMENT_3D('',#12886,#10326,#10327);
#8947=AXIS2_PLACEMENT_3D('',#12887,#10328,#10329);
#8948=AXIS2_PLACEMENT_3D('',#12889,#10330,#10331);
#8949=AXIS2_PLACEMENT_3D('',#12892,#10333,#10334);
#8950=AXIS2_PLACEMENT_3D('',#12893,#10335,#10336);
#8951=AXIS2_PLACEMENT_3D('',#12902,#10341,#10342);
#8952=AXIS2_PLACEMENT_3D('',#12911,#10347,#10348);
#8953=AXIS2_PLACEMENT_3D('',#12917,#10352,#10353);
#8954=AXIS2_PLACEMENT_3D('',#12923,#10357,#10358);
#8955=AXIS2_PLACEMENT_3D('',#12930,#10363,#10364);
#8956=AXIS2_PLACEMENT_3D('',#12934,#10367,#10368);
#8957=AXIS2_PLACEMENT_3D('',#12939,#10372,#10373);
#8958=AXIS2_PLACEMENT_3D('',#12941,#10375,#10376);
#8959=AXIS2_PLACEMENT_3D('',#12942,#10377,#10378);
#8960=AXIS2_PLACEMENT_3D('',#12943,#10379,#10380);
#8961=AXIS2_PLACEMENT_3D('',#12944,#10381,#10382);
#8962=AXIS2_PLACEMENT_3D('',#12946,#10383,#10384);
#8963=AXIS2_PLACEMENT_3D('',#12949,#10386,#10387);
#8964=AXIS2_PLACEMENT_3D('',#12950,#10388,#10389);
#8965=AXIS2_PLACEMENT_3D('',#12952,#10390,#10391);
#8966=AXIS2_PLACEMENT_3D('',#12955,#10393,#10394);
#8967=AXIS2_PLACEMENT_3D('',#12956,#10395,#10396);
#8968=AXIS2_PLACEMENT_3D('',#12958,#10397,#10398);
#8969=AXIS2_PLACEMENT_3D('',#12961,#10400,#10401);
#8970=AXIS2_PLACEMENT_3D('',#12962,#10402,#10403);
#8971=AXIS2_PLACEMENT_3D('',#12964,#10404,#10405);
#8972=AXIS2_PLACEMENT_3D('',#12967,#10407,#10408);
#8973=AXIS2_PLACEMENT_3D('',#12968,#10409,#10410);
#8974=AXIS2_PLACEMENT_3D('',#12970,#10411,#10412);
#8975=AXIS2_PLACEMENT_3D('',#12973,#10414,#10415);
#8976=AXIS2_PLACEMENT_3D('',#12974,#10416,#10417);
#8977=AXIS2_PLACEMENT_3D('',#12976,#10418,#10419);
#8978=AXIS2_PLACEMENT_3D('',#12977,#10420,#10421);
#8979=AXIS2_PLACEMENT_3D('',#12980,#10423,#10424);
#8980=AXIS2_PLACEMENT_3D('',#12981,#10425,#10426);
#8981=AXIS2_PLACEMENT_3D('',#12983,#10427,#10428);
#8982=AXIS2_PLACEMENT_3D('',#12986,#10430,#10431);
#8983=AXIS2_PLACEMENT_3D('',#12987,#10432,#10433);
#8984=AXIS2_PLACEMENT_3D('',#12988,#10434,#10435);
#8985=AXIS2_PLACEMENT_3D('',#12989,#10436,#10437);
#8986=AXIS2_PLACEMENT_3D('',#12990,#10438,#10439);
#8987=AXIS2_PLACEMENT_3D('',#12992,#10440,#10441);
#8988=AXIS2_PLACEMENT_3D('',#12995,#10443,#10444);
#8989=AXIS2_PLACEMENT_3D('',#12996,#10445,#10446);
#8990=AXIS2_PLACEMENT_3D('',#12998,#10447,#10448);
#8991=AXIS2_PLACEMENT_3D('',#13001,#10450,#10451);
#8992=AXIS2_PLACEMENT_3D('',#13002,#10452,#10453);
#8993=AXIS2_PLACEMENT_3D('',#13004,#10454,#10455);
#8994=AXIS2_PLACEMENT_3D('',#13007,#10457,#10458);
#8995=AXIS2_PLACEMENT_3D('',#13008,#10459,#10460);
#8996=AXIS2_PLACEMENT_3D('',#13010,#10461,#10462);
#8997=AXIS2_PLACEMENT_3D('',#13013,#10464,#10465);
#8998=AXIS2_PLACEMENT_3D('',#13014,#10466,#10467);
#8999=AXIS2_PLACEMENT_3D('',#13016,#10468,#10469);
#9000=AXIS2_PLACEMENT_3D('',#13019,#10471,#10472);
#9001=AXIS2_PLACEMENT_3D('',#13020,#10473,#10474);
#9002=AXIS2_PLACEMENT_3D('',#13022,#10475,#10476);
#9003=AXIS2_PLACEMENT_3D('',#13023,#10477,#10478);
#9004=AXIS2_PLACEMENT_3D('',#13025,#10479,#10480);
#9005=AXIS2_PLACEMENT_3D('',#13027,#10482,#10483);
#9006=AXIS2_PLACEMENT_3D('',#13029,#10484,#10485);
#9007=AXIS2_PLACEMENT_3D('',#13032,#10487,#10488);
#9008=AXIS2_PLACEMENT_3D('',#13033,#10489,#10490);
#9009=AXIS2_PLACEMENT_3D('',#13034,#10491,#10492);
#9010=AXIS2_PLACEMENT_3D('',#13035,#10493,#10494);
#9011=AXIS2_PLACEMENT_3D('',#13036,#10495,#10496);
#9012=AXIS2_PLACEMENT_3D('',#13038,#10497,#10498);
#9013=AXIS2_PLACEMENT_3D('',#13041,#10500,#10501);
#9014=AXIS2_PLACEMENT_3D('',#13042,#10502,#10503);
#9015=AXIS2_PLACEMENT_3D('',#13044,#10504,#10505);
#9016=AXIS2_PLACEMENT_3D('',#13047,#10507,#10508);
#9017=AXIS2_PLACEMENT_3D('',#13048,#10509,#10510);
#9018=AXIS2_PLACEMENT_3D('',#13050,#10511,#10512);
#9019=AXIS2_PLACEMENT_3D('',#13053,#10514,#10515);
#9020=AXIS2_PLACEMENT_3D('',#13054,#10516,#10517);
#9021=AXIS2_PLACEMENT_3D('',#13056,#10518,#10519);
#9022=AXIS2_PLACEMENT_3D('',#13059,#10521,#10522);
#9023=AXIS2_PLACEMENT_3D('',#13060,#10523,#10524);
#9024=AXIS2_PLACEMENT_3D('',#13062,#10525,#10526);
#9025=AXIS2_PLACEMENT_3D('',#13065,#10528,#10529);
#9026=AXIS2_PLACEMENT_3D('',#13066,#10530,#10531);
#9027=AXIS2_PLACEMENT_3D('',#13068,#10532,#10533);
#9028=AXIS2_PLACEMENT_3D('',#13071,#10535,#10536);
#9029=AXIS2_PLACEMENT_3D('',#13072,#10537,#10538);
#9030=AXIS2_PLACEMENT_3D('',#13074,#10539,#10540);
#9031=AXIS2_PLACEMENT_3D('',#13077,#10542,#10543);
#9032=AXIS2_PLACEMENT_3D('',#13078,#10544,#10545);
#9033=AXIS2_PLACEMENT_3D('',#13087,#10550,#10551);
#9034=AXIS2_PLACEMENT_3D('',#13096,#10556,#10557);
#9035=AXIS2_PLACEMENT_3D('',#13102,#10561,#10562);
#9036=AXIS2_PLACEMENT_3D('',#13108,#10566,#10567);
#9037=AXIS2_PLACEMENT_3D('',#13115,#10572,#10573);
#9038=AXIS2_PLACEMENT_3D('',#13119,#10576,#10577);
#9039=AXIS2_PLACEMENT_3D('',#13124,#10581,#10582);
#9040=AXIS2_PLACEMENT_3D('',#13126,#10584,#10585);
#9041=AXIS2_PLACEMENT_3D('',#13127,#10586,#10587);
#9042=AXIS2_PLACEMENT_3D('',#13128,#10588,#10589);
#9043=AXIS2_PLACEMENT_3D('',#13129,#10590,#10591);
#9044=AXIS2_PLACEMENT_3D('',#13131,#10592,#10593);
#9045=AXIS2_PLACEMENT_3D('',#13134,#10595,#10596);
#9046=AXIS2_PLACEMENT_3D('',#13135,#10597,#10598);
#9047=AXIS2_PLACEMENT_3D('',#13137,#10599,#10600);
#9048=AXIS2_PLACEMENT_3D('',#13140,#10602,#10603);
#9049=AXIS2_PLACEMENT_3D('',#13141,#10604,#10605);
#9050=AXIS2_PLACEMENT_3D('',#13143,#10606,#10607);
#9051=AXIS2_PLACEMENT_3D('',#13146,#10609,#10610);
#9052=AXIS2_PLACEMENT_3D('',#13147,#10611,#10612);
#9053=AXIS2_PLACEMENT_3D('',#13149,#10613,#10614);
#9054=AXIS2_PLACEMENT_3D('',#13152,#10616,#10617);
#9055=AXIS2_PLACEMENT_3D('',#13153,#10618,#10619);
#9056=AXIS2_PLACEMENT_3D('',#13155,#10620,#10621);
#9057=AXIS2_PLACEMENT_3D('',#13158,#10623,#10624);
#9058=AXIS2_PLACEMENT_3D('',#13159,#10625,#10626);
#9059=AXIS2_PLACEMENT_3D('',#13161,#10627,#10628);
#9060=AXIS2_PLACEMENT_3D('',#13162,#10629,#10630);
#9061=AXIS2_PLACEMENT_3D('',#13165,#10632,#10633);
#9062=AXIS2_PLACEMENT_3D('',#13166,#10634,#10635);
#9063=AXIS2_PLACEMENT_3D('',#13168,#10636,#10637);
#9064=AXIS2_PLACEMENT_3D('',#13171,#10639,#10640);
#9065=AXIS2_PLACEMENT_3D('',#13172,#10641,#10642);
#9066=AXIS2_PLACEMENT_3D('',#13173,#10643,#10644);
#9067=AXIS2_PLACEMENT_3D('',#13174,#10645,#10646);
#9068=AXIS2_PLACEMENT_3D('',#13175,#10647,#10648);
#9069=AXIS2_PLACEMENT_3D('',#13177,#10649,#10650);
#9070=AXIS2_PLACEMENT_3D('',#13180,#10652,#10653);
#9071=AXIS2_PLACEMENT_3D('',#13181,#10654,#10655);
#9072=AXIS2_PLACEMENT_3D('',#13183,#10656,#10657);
#9073=AXIS2_PLACEMENT_3D('',#13186,#10659,#10660);
#9074=AXIS2_PLACEMENT_3D('',#13187,#10661,#10662);
#9075=AXIS2_PLACEMENT_3D('',#13189,#10663,#10664);
#9076=AXIS2_PLACEMENT_3D('',#13192,#10666,#10667);
#9077=AXIS2_PLACEMENT_3D('',#13193,#10668,#10669);
#9078=AXIS2_PLACEMENT_3D('',#13195,#10670,#10671);
#9079=AXIS2_PLACEMENT_3D('',#13198,#10673,#10674);
#9080=AXIS2_PLACEMENT_3D('',#13199,#10675,#10676);
#9081=AXIS2_PLACEMENT_3D('',#13201,#10677,#10678);
#9082=AXIS2_PLACEMENT_3D('',#13204,#10680,#10681);
#9083=AXIS2_PLACEMENT_3D('',#13205,#10682,#10683);
#9084=AXIS2_PLACEMENT_3D('',#13207,#10684,#10685);
#9085=AXIS2_PLACEMENT_3D('',#13208,#10686,#10687);
#9086=AXIS2_PLACEMENT_3D('',#13210,#10688,#10689);
#9087=AXIS2_PLACEMENT_3D('',#13212,#10691,#10692);
#9088=AXIS2_PLACEMENT_3D('',#13214,#10693,#10694);
#9089=AXIS2_PLACEMENT_3D('',#13217,#10696,#10697);
#9090=AXIS2_PLACEMENT_3D('',#13218,#10698,#10699);
#9091=AXIS2_PLACEMENT_3D('',#13219,#10700,#10701);
#9092=AXIS2_PLACEMENT_3D('',#13220,#10702,#10703);
#9093=AXIS2_PLACEMENT_3D('',#13221,#10704,#10705);
#9094=AXIS2_PLACEMENT_3D('',#13223,#10706,#10707);
#9095=AXIS2_PLACEMENT_3D('',#13226,#10709,#10710);
#9096=AXIS2_PLACEMENT_3D('',#13227,#10711,#10712);
#9097=AXIS2_PLACEMENT_3D('',#13229,#10713,#10714);
#9098=AXIS2_PLACEMENT_3D('',#13232,#10716,#10717);
#9099=AXIS2_PLACEMENT_3D('',#13233,#10718,#10719);
#9100=AXIS2_PLACEMENT_3D('',#13235,#10720,#10721);
#9101=AXIS2_PLACEMENT_3D('',#13238,#10723,#10724);
#9102=AXIS2_PLACEMENT_3D('',#13239,#10725,#10726);
#9103=AXIS2_PLACEMENT_3D('',#13241,#10727,#10728);
#9104=AXIS2_PLACEMENT_3D('',#13244,#10730,#10731);
#9105=AXIS2_PLACEMENT_3D('',#13245,#10732,#10733);
#9106=AXIS2_PLACEMENT_3D('',#13247,#10734,#10735);
#9107=AXIS2_PLACEMENT_3D('',#13250,#10737,#10738);
#9108=AXIS2_PLACEMENT_3D('',#13251,#10739,#10740);
#9109=AXIS2_PLACEMENT_3D('',#13253,#10741,#10742);
#9110=AXIS2_PLACEMENT_3D('',#13256,#10744,#10745);
#9111=AXIS2_PLACEMENT_3D('',#13257,#10746,#10747);
#9112=AXIS2_PLACEMENT_3D('',#13259,#10748,#10749);
#9113=AXIS2_PLACEMENT_3D('',#13262,#10751,#10752);
#9114=AXIS2_PLACEMENT_3D('',#13263,#10753,#10754);
#9115=AXIS2_PLACEMENT_3D('',#13272,#10759,#10760);
#9116=AXIS2_PLACEMENT_3D('',#13281,#10765,#10766);
#9117=AXIS2_PLACEMENT_3D('',#13287,#10770,#10771);
#9118=AXIS2_PLACEMENT_3D('',#13293,#10775,#10776);
#9119=AXIS2_PLACEMENT_3D('',#13300,#10781,#10782);
#9120=AXIS2_PLACEMENT_3D('',#13304,#10785,#10786);
#9121=AXIS2_PLACEMENT_3D('',#13309,#10790,#10791);
#9122=AXIS2_PLACEMENT_3D('',#13311,#10793,#10794);
#9123=AXIS2_PLACEMENT_3D('',#13312,#10795,#10796);
#9124=AXIS2_PLACEMENT_3D('',#13313,#10797,#10798);
#9125=AXIS2_PLACEMENT_3D('',#13314,#10799,#10800);
#9126=AXIS2_PLACEMENT_3D('',#13316,#10801,#10802);
#9127=AXIS2_PLACEMENT_3D('',#13319,#10804,#10805);
#9128=AXIS2_PLACEMENT_3D('',#13320,#10806,#10807);
#9129=AXIS2_PLACEMENT_3D('',#13322,#10808,#10809);
#9130=AXIS2_PLACEMENT_3D('',#13325,#10811,#10812);
#9131=AXIS2_PLACEMENT_3D('',#13326,#10813,#10814);
#9132=AXIS2_PLACEMENT_3D('',#13328,#10815,#10816);
#9133=AXIS2_PLACEMENT_3D('',#13331,#10818,#10819);
#9134=AXIS2_PLACEMENT_3D('',#13332,#10820,#10821);
#9135=AXIS2_PLACEMENT_3D('',#13334,#10822,#10823);
#9136=AXIS2_PLACEMENT_3D('',#13337,#10825,#10826);
#9137=AXIS2_PLACEMENT_3D('',#13338,#10827,#10828);
#9138=AXIS2_PLACEMENT_3D('',#13340,#10829,#10830);
#9139=AXIS2_PLACEMENT_3D('',#13343,#10832,#10833);
#9140=AXIS2_PLACEMENT_3D('',#13344,#10834,#10835);
#9141=AXIS2_PLACEMENT_3D('',#13346,#10836,#10837);
#9142=AXIS2_PLACEMENT_3D('',#13347,#10838,#10839);
#9143=AXIS2_PLACEMENT_3D('',#13350,#10841,#10842);
#9144=AXIS2_PLACEMENT_3D('',#13351,#10843,#10844);
#9145=AXIS2_PLACEMENT_3D('',#13353,#10845,#10846);
#9146=AXIS2_PLACEMENT_3D('',#13356,#10848,#10849);
#9147=AXIS2_PLACEMENT_3D('',#13357,#10850,#10851);
#9148=AXIS2_PLACEMENT_3D('',#13358,#10852,#10853);
#9149=AXIS2_PLACEMENT_3D('',#13359,#10854,#10855);
#9150=AXIS2_PLACEMENT_3D('',#13360,#10856,#10857);
#9151=AXIS2_PLACEMENT_3D('',#13362,#10858,#10859);
#9152=AXIS2_PLACEMENT_3D('',#13365,#10861,#10862);
#9153=AXIS2_PLACEMENT_3D('',#13366,#10863,#10864);
#9154=AXIS2_PLACEMENT_3D('',#13368,#10865,#10866);
#9155=AXIS2_PLACEMENT_3D('',#13371,#10868,#10869);
#9156=AXIS2_PLACEMENT_3D('',#13372,#10870,#10871);
#9157=AXIS2_PLACEMENT_3D('',#13374,#10872,#10873);
#9158=AXIS2_PLACEMENT_3D('',#13377,#10875,#10876);
#9159=AXIS2_PLACEMENT_3D('',#13378,#10877,#10878);
#9160=AXIS2_PLACEMENT_3D('',#13380,#10879,#10880);
#9161=AXIS2_PLACEMENT_3D('',#13383,#10882,#10883);
#9162=AXIS2_PLACEMENT_3D('',#13384,#10884,#10885);
#9163=AXIS2_PLACEMENT_3D('',#13386,#10886,#10887);
#9164=AXIS2_PLACEMENT_3D('',#13389,#10889,#10890);
#9165=AXIS2_PLACEMENT_3D('',#13390,#10891,#10892);
#9166=AXIS2_PLACEMENT_3D('',#13392,#10893,#10894);
#9167=AXIS2_PLACEMENT_3D('',#13393,#10895,#10896);
#9168=AXIS2_PLACEMENT_3D('',#13395,#10897,#10898);
#9169=AXIS2_PLACEMENT_3D('',#13397,#10900,#10901);
#9170=AXIS2_PLACEMENT_3D('',#13399,#10902,#10903);
#9171=AXIS2_PLACEMENT_3D('',#13402,#10905,#10906);
#9172=AXIS2_PLACEMENT_3D('',#13403,#10907,#10908);
#9173=AXIS2_PLACEMENT_3D('',#13404,#10909,#10910);
#9174=AXIS2_PLACEMENT_3D('',#13405,#10911,#10912);
#9175=AXIS2_PLACEMENT_3D('',#13406,#10913,#10914);
#9176=AXIS2_PLACEMENT_3D('',#13408,#10915,#10916);
#9177=AXIS2_PLACEMENT_3D('',#13411,#10918,#10919);
#9178=AXIS2_PLACEMENT_3D('',#13412,#10920,#10921);
#9179=AXIS2_PLACEMENT_3D('',#13414,#10922,#10923);
#9180=AXIS2_PLACEMENT_3D('',#13417,#10925,#10926);
#9181=AXIS2_PLACEMENT_3D('',#13418,#10927,#10928);
#9182=AXIS2_PLACEMENT_3D('',#13420,#10929,#10930);
#9183=AXIS2_PLACEMENT_3D('',#13423,#10932,#10933);
#9184=AXIS2_PLACEMENT_3D('',#13424,#10934,#10935);
#9185=AXIS2_PLACEMENT_3D('',#13426,#10936,#10937);
#9186=AXIS2_PLACEMENT_3D('',#13427,#10938,#10939);
#9187=AXIS2_PLACEMENT_3D('',#13429,#10940,#10941);
#9188=AXIS2_PLACEMENT_3D('',#13431,#10943,#10944);
#9189=AXIS2_PLACEMENT_3D('',#13433,#10945,#10946);
#9190=AXIS2_PLACEMENT_3D('',#13436,#10948,#10949);
#9191=AXIS2_PLACEMENT_3D('',#13437,#10950,#10951);
#9192=AXIS2_PLACEMENT_3D('',#13439,#10952,#10953);
#9193=AXIS2_PLACEMENT_3D('',#13440,#10954,#10955);
#9194=AXIS2_PLACEMENT_3D('',#13442,#10956,#10957);
#9195=AXIS2_PLACEMENT_3D('',#13444,#10959,#10960);
#9196=AXIS2_PLACEMENT_3D('',#13453,#10965,#10966);
#9197=AXIS2_PLACEMENT_3D('',#13459,#10970,#10971);
#9198=AXIS2_PLACEMENT_3D('',#13465,#10975,#10976);
#9199=AXIS2_PLACEMENT_3D('',#13468,#10979,#10980);
#9200=AXIS2_PLACEMENT_3D('',#13469,#10981,#10982);
#9201=AXIS2_PLACEMENT_3D('',#13470,#10983,#10984);
#9202=AXIS2_PLACEMENT_3D('',#13471,#10985,#10986);
#9203=AXIS2_PLACEMENT_3D('',#13473,#10987,#10988);
#9204=AXIS2_PLACEMENT_3D('',#13476,#10990,#10991);
#9205=AXIS2_PLACEMENT_3D('',#13477,#10992,#10993);
#9206=AXIS2_PLACEMENT_3D('',#13478,#10994,#10995);
#9207=AXIS2_PLACEMENT_3D('',#13479,#10996,#10997);
#9208=AXIS2_PLACEMENT_3D('',#13480,#10998,#10999);
#9209=AXIS2_PLACEMENT_3D('',#13482,#11000,#11001);
#9210=AXIS2_PLACEMENT_3D('',#13485,#11003,#11004);
#9211=AXIS2_PLACEMENT_3D('',#13486,#11005,#11006);
#9212=AXIS2_PLACEMENT_3D('',#13487,#11007,#11008);
#9213=AXIS2_PLACEMENT_3D('',#13488,#11009,#11010);
#9214=AXIS2_PLACEMENT_3D('',#14320,#11011,#11012);
#9215=AXIS2_PLACEMENT_3D('',#14405,#11013,#11014);
#9216=AXIS2_PLACEMENT_3D('',#14406,#11015,#11016);
#9217=AXIS2_PLACEMENT_3D('',#14407,#11017,#11018);
#9218=AXIS2_PLACEMENT_3D('',#14408,#11019,#11020);
#9219=AXIS2_PLACEMENT_3D('',#14409,#11021,#11022);
#9220=AXIS2_PLACEMENT_3D('',#14411,#11023,#11024);
#9221=AXIS2_PLACEMENT_3D('',#14414,#11026,#11027);
#9222=AXIS2_PLACEMENT_3D('',#14415,#11028,#11029);
#9223=AXIS2_PLACEMENT_3D('',#14416,#11030,#11031);
#9224=AXIS2_PLACEMENT_3D('',#14417,#11032,#11033);
#9225=AXIS2_PLACEMENT_3D('',#14418,#11034,#11035);
#9226=AXIS2_PLACEMENT_3D('',#14420,#11036,#11037);
#9227=AXIS2_PLACEMENT_3D('',#14423,#11039,#11040);
#9228=AXIS2_PLACEMENT_3D('',#14424,#11041,#11042);
#9229=AXIS2_PLACEMENT_3D('',#14425,#11043,#11044);
#9230=AXIS2_PLACEMENT_3D('',#14426,#11045,#11046);
#9231=AXIS2_PLACEMENT_3D('',#15238,#11047,#11048);
#9232=AXIS2_PLACEMENT_3D('',#15321,#11049,#11050);
#9233=AXIS2_PLACEMENT_3D('',#15322,#11051,#11052);
#9234=AXIS2_PLACEMENT_3D('',#15323,#11053,#11054);
#9235=AXIS2_PLACEMENT_3D('',#15324,#11055,#11056);
#9236=AXIS2_PLACEMENT_3D('',#15325,#11057,#11058);
#9237=AXIS2_PLACEMENT_3D('',#15327,#11059,#11060);
#9238=AXIS2_PLACEMENT_3D('',#15328,#11061,#11062);
#9239=AXIS2_PLACEMENT_3D('',#15330,#11063,#11064);
#9240=AXIS2_PLACEMENT_3D('',#15332,#11066,#11067);
#9241=AXIS2_PLACEMENT_3D('',#15334,#11068,#11069);
#9242=AXIS2_PLACEMENT_3D('',#15336,#11071,#11072);
#9243=AXIS2_PLACEMENT_3D('',#15338,#11073,#11074);
#9244=AXIS2_PLACEMENT_3D('',#15340,#11076,#11077);
#9245=AXIS2_PLACEMENT_3D('',#15342,#11078,#11079);
#9246=AXIS2_PLACEMENT_3D('',#15343,#11080,#11081);
#9247=AXIS2_PLACEMENT_3D('',#15345,#11082,#11083);
#9248=AXIS2_PLACEMENT_3D('',#15347,#11085,#11086);
#9249=AXIS2_PLACEMENT_3D('',#15349,#11087,#11088);
#9250=AXIS2_PLACEMENT_3D('',#15351,#11090,#11091);
#9251=AXIS2_PLACEMENT_3D('',#15353,#11092,#11093);
#9252=AXIS2_PLACEMENT_3D('',#15355,#11095,#11096);
#9253=AXIS2_PLACEMENT_3D('',#15356,#11097,#11098);
#9254=AXIS2_PLACEMENT_3D('',#15365,#11103,#11104);
#9255=AXIS2_PLACEMENT_3D('',#15371,#11108,#11109);
#9256=AXIS2_PLACEMENT_3D('',#15377,#11113,#11114);
#9257=AXIS2_PLACEMENT_3D('',#15383,#11118,#11119);
#9258=AXIS2_PLACEMENT_3D('',#15389,#11123,#11124);
#9259=AXIS2_PLACEMENT_3D('',#15392,#11127,#11128);
#9260=AXIS2_PLACEMENT_3D('',#15393,#11129,#11130);
#9261=AXIS2_PLACEMENT_3D('',#15394,#11131,#11132);
#9262=AXIS2_PLACEMENT_3D('',#15395,#11133,#11134);
#9263=AXIS2_PLACEMENT_3D('',#15396,#11135,#11136);
#9264=AXIS2_PLACEMENT_3D('',#15399,#11137,#11138);
#9265=AXIS2_PLACEMENT_3D('',#15400,#11139,#11140);
#9266=AXIS2_PLACEMENT_3D('',#15402,#11141,#11142);
#9267=AXIS2_PLACEMENT_3D('',#15404,#11143,#11144);
#9268=AXIS2_PLACEMENT_3D('',#15405,#11145,#11146);
#9269=AXIS2_PLACEMENT_3D('',#15406,#11147,#11148);
#9270=AXIS2_PLACEMENT_3D('',#15409,#11150,#11151);
#9271=AXIS2_PLACEMENT_3D('',#15410,#11152,#11153);
#9272=AXIS2_PLACEMENT_3D('',#15412,#11154,#11155);
#9273=AXIS2_PLACEMENT_3D('',#15415,#11157,#11158);
#9274=AXIS2_PLACEMENT_3D('',#15416,#11159,#11160);
#9275=AXIS2_PLACEMENT_3D('',#15419,#11162,#11163);
#9276=AXIS2_PLACEMENT_3D('',#15420,#11164,#11165);
#9277=AXIS2_PLACEMENT_3D('',#15421,#11166,#11167);
#9278=AXIS2_PLACEMENT_3D('',#15423,#11168,#11169);
#9279=AXIS2_PLACEMENT_3D('',#15425,#11171,#11172);
#9280=AXIS2_PLACEMENT_3D('',#15427,#11173,#11174);
#9281=AXIS2_PLACEMENT_3D('',#15428,#11175,#11176);
#9282=AXIS2_PLACEMENT_3D('',#15430,#11178,#11179);
#9283=AXIS2_PLACEMENT_3D('',#15431,#11180,#11181);
#9284=AXIS2_PLACEMENT_3D('',#15434,#11182,#11183);
#9285=AXIS2_PLACEMENT_3D('',#15435,#11184,#11185);
#9286=AXIS2_PLACEMENT_3D('',#15437,#11186,#11187);
#9287=AXIS2_PLACEMENT_3D('',#15439,#11188,#11189);
#9288=AXIS2_PLACEMENT_3D('',#15440,#11190,#11191);
#9289=AXIS2_PLACEMENT_3D('',#15441,#11192,#11193);
#9290=AXIS2_PLACEMENT_3D('',#15443,#11194,#11195);
#9291=AXIS2_PLACEMENT_3D('',#15445,#11197,#11198);
#9292=AXIS2_PLACEMENT_3D('',#15447,#11199,#11200);
#9293=AXIS2_PLACEMENT_3D('',#15449,#11201,#11202);
#9294=AXIS2_PLACEMENT_3D('',#15450,#11203,#11204);
#9295=AXIS2_PLACEMENT_3D('',#15452,#11205,#11206);
#9296=AXIS2_PLACEMENT_3D('',#15454,#11208,#11209);
#9297=AXIS2_PLACEMENT_3D('',#15456,#11210,#11211);
#9298=AXIS2_PLACEMENT_3D('',#15458,#11213,#11214);
#9299=AXIS2_PLACEMENT_3D('',#15460,#11215,#11216);
#9300=AXIS2_PLACEMENT_3D('',#15462,#11218,#11219);
#9301=AXIS2_PLACEMENT_3D('',#15463,#11220,#11221);
#9302=AXIS2_PLACEMENT_3D('',#15465,#11223,#11224);
#9303=AXIS2_PLACEMENT_3D('',#15466,#11225,#11226);
#9304=AXIS2_PLACEMENT_3D('',#15469,#11227,#11228);
#9305=AXIS2_PLACEMENT_3D('',#15470,#11229,#11230);
#9306=AXIS2_PLACEMENT_3D('',#15473,#11231,#11232);
#9307=AXIS2_PLACEMENT_3D('',#15474,#11233,#11234);
#9308=AXIS2_PLACEMENT_3D('',#15477,#11235,#11236);
#9309=AXIS2_PLACEMENT_3D('',#15478,#11237,#11238);
#9310=AXIS2_PLACEMENT_3D('',#15481,#11239,#11240);
#9311=AXIS2_PLACEMENT_3D('',#15482,#11241,#11242);
#9312=AXIS2_PLACEMENT_3D('',#15485,#11243,#11244);
#9313=AXIS2_PLACEMENT_3D('',#15486,#11245,#11246);
#9314=AXIS2_PLACEMENT_3D('',#15489,#11247,#11248);
#9315=AXIS2_PLACEMENT_3D('',#15490,#11249,#11250);
#9316=AXIS2_PLACEMENT_3D('',#15493,#11251,#11252);
#9317=AXIS2_PLACEMENT_3D('',#15494,#11253,#11254);
#9318=AXIS2_PLACEMENT_3D('',#15495,#11255,#11256);
#9319=AXIS2_PLACEMENT_3D('',#15521,#11257,#11258);
#9320=AXIS2_PLACEMENT_3D('',#15545,#11259,#11260);
#9321=AXIS2_PLACEMENT_3D('',#15546,#11261,#11262);
#9322=AXIS2_PLACEMENT_3D('',#15548,#11263,#11264);
#9323=AXIS2_PLACEMENT_3D('',#15573,#11265,#11266);
#9324=AXIS2_PLACEMENT_3D('',#15598,#11267,#11268);
#9325=AXIS2_PLACEMENT_3D('',#15601,#11270,#11271);
#9326=AXIS2_PLACEMENT_3D('',#15603,#11272,#11273);
#9327=AXIS2_PLACEMENT_3D('',#15628,#11274,#11275);
#9328=AXIS2_PLACEMENT_3D('',#15653,#11276,#11277);
#9329=AXIS2_PLACEMENT_3D('',#15678,#11278,#11279);
#9330=AXIS2_PLACEMENT_3D('',#15702,#11280,#11281);
#9331=AXIS2_PLACEMENT_3D('',#15703,#11282,#11283);
#9332=AXIS2_PLACEMENT_3D('',#15705,#11284,#11285);
#9333=AXIS2_PLACEMENT_3D('',#15706,#11286,#11287);
#9334=AXIS2_PLACEMENT_3D('',#15707,#11288,#11289);
#9335=AXIS2_PLACEMENT_3D('',#15731,#11290,#11291);
#9336=AXIS2_PLACEMENT_3D('',#15732,#11292,#11293);
#9337=AXIS2_PLACEMENT_3D('',#15734,#11294,#11295);
#9338=AXIS2_PLACEMENT_3D('',#15735,#11296,#11297);
#9339=AXIS2_PLACEMENT_3D('',#15736,#11298,#11299);
#9340=AXIS2_PLACEMENT_3D('',#15760,#11300,#11301);
#9341=AXIS2_PLACEMENT_3D('',#15761,#11302,#11303);
#9342=AXIS2_PLACEMENT_3D('',#15763,#11304,#11305);
#9343=AXIS2_PLACEMENT_3D('',#15765,#11306,#11307);
#9344=AXIS2_PLACEMENT_3D('',#15766,#11308,#11309);
#9345=AXIS2_PLACEMENT_3D('',#15767,#11310,#11311);
#9346=AXIS2_PLACEMENT_3D('',#15791,#11312,#11313);
#9347=AXIS2_PLACEMENT_3D('',#15792,#11314,#11315);
#9348=AXIS2_PLACEMENT_3D('',#15794,#11316,#11317);
#9349=AXIS2_PLACEMENT_3D('',#15795,#11318,#11319);
#9350=AXIS2_PLACEMENT_3D('',#15796,#11320,#11321);
#9351=AXIS2_PLACEMENT_3D('',#15820,#11322,#11323);
#9352=AXIS2_PLACEMENT_3D('',#15821,#11324,#11325);
#9353=AXIS2_PLACEMENT_3D('',#15823,#11326,#11327);
#9354=AXIS2_PLACEMENT_3D('',#15824,#11328,#11329);
#9355=AXIS2_PLACEMENT_3D('',#15825,#11330,#11331);
#9356=AXIS2_PLACEMENT_3D('',#15849,#11332,#11333);
#9357=AXIS2_PLACEMENT_3D('',#15850,#11334,#11335);
#9358=AXIS2_PLACEMENT_3D('',#15852,#11336,#11337);
#9359=AXIS2_PLACEMENT_3D('',#15855,#11339,#11340);
#9360=AXIS2_PLACEMENT_3D('',#15879,#11341,#11342);
#9361=AXIS2_PLACEMENT_3D('',#15880,#11343,#11344);
#9362=AXIS2_PLACEMENT_3D('',#15881,#11345,#11346);
#9363=AXIS2_PLACEMENT_3D('',#15882,#11347,#11348);
#9364=AXIS2_PLACEMENT_3D('',#15883,#11349,#11350);
#9365=AXIS2_PLACEMENT_3D('',#15884,#11351,#11352);
#9366=AXIS2_PLACEMENT_3D('',#15885,#11353,#11354);
#9367=AXIS2_PLACEMENT_3D('',#15886,#11355,#11356);
#9368=AXIS2_PLACEMENT_3D('',#15887,#11357,#11358);
#9369=AXIS2_PLACEMENT_3D('',#15889,#11359,#11360);
#9370=AXIS2_PLACEMENT_3D('',#15891,#11361,#11362);
#9371=AXIS2_PLACEMENT_3D('',#15892,#11363,#11364);
#9372=AXIS2_PLACEMENT_3D('',#15894,#11365,#11366);
#9373=AXIS2_PLACEMENT_3D('',#15896,#11368,#11369);
#9374=AXIS2_PLACEMENT_3D('',#15898,#11370,#11371);
#9375=AXIS2_PLACEMENT_3D('',#15899,#11372,#11373);
#9376=AXIS2_PLACEMENT_3D('',#15901,#11375,#11376);
#9377=AXIS2_PLACEMENT_3D('',#15903,#11377,#11378);
#9378=AXIS2_PLACEMENT_3D('',#15905,#11379,#11380);
#9379=AXIS2_PLACEMENT_3D('',#15906,#11381,#11382);
#9380=AXIS2_PLACEMENT_3D('',#15908,#11383,#11384);
#9381=AXIS2_PLACEMENT_3D('',#15910,#11386,#11387);
#9382=AXIS2_PLACEMENT_3D('',#15912,#11388,#11389);
#9383=AXIS2_PLACEMENT_3D('',#15913,#11390,#11391);
#9384=AXIS2_PLACEMENT_3D('',#15915,#11393,#11394);
#9385=AXIS2_PLACEMENT_3D('',#15916,#11395,#11396);
#9386=AXIS2_PLACEMENT_3D('',#15917,#11397,#11398);
#9387=AXIS2_PLACEMENT_3D('',#15918,#11399,#11400);
#9388=AXIS2_PLACEMENT_3D('',#15919,#11401,#11402);
#9389=AXIS2_PLACEMENT_3D('',#15920,#11403,#11404);
#9390=AXIS2_PLACEMENT_3D('',#15921,#11405,#11406);
#9391=AXIS2_PLACEMENT_3D('',#15930,#11411,#11412);
#9392=AXIS2_PLACEMENT_3D('',#15936,#11416,#11417);
#9393=AXIS2_PLACEMENT_3D('',#15942,#11421,#11422);
#9394=AXIS2_PLACEMENT_3D('',#15948,#11426,#11427);
#9395=AXIS2_PLACEMENT_3D('',#15954,#11431,#11432);
#9396=AXIS2_PLACEMENT_3D('',#15957,#11435,#11436);
#9397=AXIS2_PLACEMENT_3D('',#15958,#11437,#11438);
#9398=AXIS2_PLACEMENT_3D('',#15959,#11439,#11440);
#9399=AXIS2_PLACEMENT_3D('',#15961,#11441,#11442);
#9400=AXIS2_PLACEMENT_3D('',#15962,#11443,#11444);
#9401=AXIS2_PLACEMENT_3D('',#15964,#11445,#11446);
#9402=AXIS2_PLACEMENT_3D('',#15965,#11447,#11448);
#9403=AXIS2_PLACEMENT_3D('',#15967,#11449,#11450);
#9404=AXIS2_PLACEMENT_3D('',#15969,#11452,#11453);
#9405=AXIS2_PLACEMENT_3D('',#15971,#11454,#11455);
#9406=AXIS2_PLACEMENT_3D('',#15973,#11457,#11458);
#9407=AXIS2_PLACEMENT_3D('',#15975,#11459,#11460);
#9408=AXIS2_PLACEMENT_3D('',#15977,#11462,#11463);
#9409=AXIS2_PLACEMENT_3D('',#15979,#11464,#11465);
#9410=AXIS2_PLACEMENT_3D('',#15980,#11466,#11467);
#9411=AXIS2_PLACEMENT_3D('',#15982,#11468,#11469);
#9412=AXIS2_PLACEMENT_3D('',#15984,#11471,#11472);
#9413=AXIS2_PLACEMENT_3D('',#15986,#11474,#11475);
#9414=AXIS2_PLACEMENT_3D('',#15987,#11476,#11477);
#9415=AXIS2_PLACEMENT_3D('',#15989,#11478,#11479);
#9416=AXIS2_PLACEMENT_3D('',#15990,#11480,#11481);
#9417=AXIS2_PLACEMENT_3D('',#15992,#11482,#11483);
#9418=AXIS2_PLACEMENT_3D('',#15994,#11485,#11486);
#9419=AXIS2_PLACEMENT_3D('',#15996,#11487,#11488);
#9420=AXIS2_PLACEMENT_3D('',#15998,#11490,#11491);
#9421=AXIS2_PLACEMENT_3D('',#16000,#11492,#11493);
#9422=AXIS2_PLACEMENT_3D('',#16002,#11495,#11496);
#9423=AXIS2_PLACEMENT_3D('',#16004,#11497,#11498);
#9424=AXIS2_PLACEMENT_3D('',#16005,#11499,#11500);
#9425=AXIS2_PLACEMENT_3D('',#16007,#11501,#11502);
#9426=AXIS2_PLACEMENT_3D('',#16009,#11504,#11505);
#9427=AXIS2_PLACEMENT_3D('',#16011,#11506,#11507);
#9428=AXIS2_PLACEMENT_3D('',#16013,#11509,#11510);
#9429=AXIS2_PLACEMENT_3D('',#16015,#11511,#11512);
#9430=AXIS2_PLACEMENT_3D('',#16017,#11514,#11515);
#9431=AXIS2_PLACEMENT_3D('',#16018,#11516,#11517);
#9432=AXIS2_PLACEMENT_3D('',#16027,#11522,#11523);
#9433=AXIS2_PLACEMENT_3D('',#16033,#11527,#11528);
#9434=AXIS2_PLACEMENT_3D('',#16039,#11532,#11533);
#9435=AXIS2_PLACEMENT_3D('',#16045,#11537,#11538);
#9436=AXIS2_PLACEMENT_3D('',#16051,#11542,#11543);
#9437=AXIS2_PLACEMENT_3D('',#16054,#11546,#11547);
#9438=AXIS2_PLACEMENT_3D('',#16055,#11548,#11549);
#9439=AXIS2_PLACEMENT_3D('',#16056,#11550,#11551);
#9440=AXIS2_PLACEMENT_3D('',#16057,#11552,#11553);
#9441=AXIS2_PLACEMENT_3D('',#16069,#11555,#11556);
#9442=AXIS2_PLACEMENT_3D('',#16085,#11557,#11558);
#9443=AXIS2_PLACEMENT_3D('',#16087,#11559,#11560);
#9444=AXIS2_PLACEMENT_3D('',#16113,#11562,#11563);
#9445=AXIS2_PLACEMENT_3D('',#16116,#11566,#11567);
#9446=AXIS2_PLACEMENT_3D('',#16118,#11569,#11570);
#9447=AXIS2_PLACEMENT_3D('',#16120,#11572,#11573);
#9448=AXIS2_PLACEMENT_3D('',#16122,#11574,#11575);
#9449=AXIS2_PLACEMENT_3D('',#16125,#11577,#11578);
#9450=AXIS2_PLACEMENT_3D('',#16126,#11579,#11580);
#9451=AXIS2_PLACEMENT_3D('',#16128,#11582,#11583);
#9452=AXIS2_PLACEMENT_3D('',#16130,#11585,#11586);
#9453=AXIS2_PLACEMENT_3D('',#16131,#11587,#11588);
#9454=AXIS2_PLACEMENT_3D('',#16132,#11589,#11590);
#9455=AXIS2_PLACEMENT_3D('',#16133,#11591,#11592);
#9456=AXIS2_PLACEMENT_3D('',#16134,#11593,#11594);
#9457=AXIS2_PLACEMENT_3D('',#16135,#11595,#11596);
#9458=AXIS2_PLACEMENT_3D('',#16137,#11597,#11598);
#9459=AXIS2_PLACEMENT_3D('',#16140,#11600,#11601);
#9460=AXIS2_PLACEMENT_3D('',#16141,#11602,#11603);
#9461=AXIS2_PLACEMENT_3D('',#16142,#11604,#11605);
#9462=AXIS2_PLACEMENT_3D('',#16151,#11610,#11611);
#9463=AXIS2_PLACEMENT_3D('',#16153,#11612,#11613);
#9464=AXIS2_PLACEMENT_3D('',#16157,#11616,#11617);
#9465=AXIS2_PLACEMENT_3D('',#16163,#11621,#11622);
#9466=AXIS2_PLACEMENT_3D('',#16165,#11624,#11625);
#9467=AXIS2_PLACEMENT_3D('',#16166,#11626,#11627);
#9468=AXIS2_PLACEMENT_3D('',#16167,#11628,#11629);
#9469=AXIS2_PLACEMENT_3D('',#16169,#11630,#11631);
#9470=AXIS2_PLACEMENT_3D('',#16171,#11632,#11633);
#9471=AXIS2_PLACEMENT_3D('',#16172,#11634,#11635);
#9472=AXIS2_PLACEMENT_3D('',#16174,#11636,#11637);
#9473=AXIS2_PLACEMENT_3D('',#16176,#11638,#11639);
#9474=AXIS2_PLACEMENT_3D('',#16177,#11640,#11641);
#9475=AXIS2_PLACEMENT_3D('',#16179,#11643,#11644);
#9476=AXIS2_PLACEMENT_3D('',#16182,#11646,#11647);
#9477=AXIS2_PLACEMENT_3D('',#16183,#11648,#11649);
#9478=AXIS2_PLACEMENT_3D('',#16185,#11650,#11651);
#9479=AXIS2_PLACEMENT_3D('',#16187,#11653,#11654);
#9480=AXIS2_PLACEMENT_3D('',#16188,#11655,#11656);
#9481=AXIS2_PLACEMENT_3D('',#16189,#11657,#11658);
#9482=AXIS2_PLACEMENT_3D('',#16190,#11659,#11660);
#9483=AXIS2_PLACEMENT_3D('',#16192,#11661,#11662);
#9484=AXIS2_PLACEMENT_3D('',#16195,#11664,#11665);
#9485=AXIS2_PLACEMENT_3D('',#16196,#11666,#11667);
#9486=AXIS2_PLACEMENT_3D('',#16198,#11668,#11669);
#9487=AXIS2_PLACEMENT_3D('',#16201,#11671,#11672);
#9488=AXIS2_PLACEMENT_3D('',#16202,#11673,#11674);
#9489=AXIS2_PLACEMENT_3D('',#16203,#11675,#11676);
#9490=AXIS2_PLACEMENT_3D('',#16204,#11677,#11678);
#9491=AXIS2_PLACEMENT_3D('',#16205,#11679,#11680);
#9492=AXIS2_PLACEMENT_3D('',#16209,#11682,#11683);
#9493=AXIS2_PLACEMENT_3D('',#16210,#11684,#11685);
#9494=AXIS2_PLACEMENT_3D('',#16223,#11686,#11687);
#9495=AXIS2_PLACEMENT_3D('',#16264,#11689,#11690);
#9496=AXIS2_PLACEMENT_3D('',#16275,#11691,#11692);
#9497=AXIS2_PLACEMENT_3D('',#16277,#11694,#11695);
#9498=AXIS2_PLACEMENT_3D('',#16279,#11696,#11697);
#9499=AXIS2_PLACEMENT_3D('',#16282,#11699,#11700);
#9500=AXIS2_PLACEMENT_3D('',#16283,#11701,#11702);
#9501=AXIS2_PLACEMENT_3D('',#16285,#11703,#11704);
#9502=AXIS2_PLACEMENT_3D('',#16288,#11706,#11707);
#9503=AXIS2_PLACEMENT_3D('',#16289,#11708,#11709);
#9504=AXIS2_PLACEMENT_3D('',#16290,#11710,#11711);
#9505=AXIS2_PLACEMENT_3D('',#16291,#11712,#11713);
#9506=AXIS2_PLACEMENT_3D('',#16292,#11714,#11715);
#9507=AXIS2_PLACEMENT_3D('',#16301,#11720,#11721);
#9508=AXIS2_PLACEMENT_3D('',#16307,#11725,#11726);
#9509=AXIS2_PLACEMENT_3D('',#16313,#11730,#11731);
#9510=AXIS2_PLACEMENT_3D('',#16315,#11732,#11733);
#9511=AXIS2_PLACEMENT_3D('',#16316,#11734,#11735);
#9512=AXIS2_PLACEMENT_3D('',#16317,#11736,#11737);
#9513=AXIS2_PLACEMENT_3D('',#16318,#11738,#11739);
#9514=AXIS2_PLACEMENT_3D('',#16319,#11740,#11741);
#9515=AXIS2_PLACEMENT_3D('',#16321,#11742,#11743);
#9516=AXIS2_PLACEMENT_3D('',#16323,#11744,#11745);
#9517=AXIS2_PLACEMENT_3D('',#16324,#11746,#11747);
#9518=AXIS2_PLACEMENT_3D('',#16326,#11749,#11750);
#9519=AXIS2_PLACEMENT_3D('',#16329,#11752,#11753);
#9520=AXIS2_PLACEMENT_3D('',#16330,#11754,#11755);
#9521=AXIS2_PLACEMENT_3D('',#16331,#11756,#11757);
#9522=AXIS2_PLACEMENT_3D('',#16332,#11758,#11759);
#9523=AXIS2_PLACEMENT_3D('',#16334,#11760,#11761);
#9524=AXIS2_PLACEMENT_3D('',#16337,#11763,#11764);
#9525=AXIS2_PLACEMENT_3D('',#16338,#11765,#11766);
#9526=AXIS2_PLACEMENT_3D('',#16340,#11767,#11768);
#9527=AXIS2_PLACEMENT_3D('',#16343,#11770,#11771);
#9528=AXIS2_PLACEMENT_3D('',#16344,#11772,#11773);
#9529=AXIS2_PLACEMENT_3D('',#16345,#11774,#11775);
#9530=AXIS2_PLACEMENT_3D('',#16346,#11776,#11777);
#9531=AXIS2_PLACEMENT_3D('',#16347,#11778,#11779);
#9532=AXIS2_PLACEMENT_3D('',#16349,#11780,#11781);
#9533=AXIS2_PLACEMENT_3D('',#16352,#11783,#11784);
#9534=AXIS2_PLACEMENT_3D('',#16353,#11785,#11786);
#9535=AXIS2_PLACEMENT_3D('',#16355,#11787,#11788);
#9536=AXIS2_PLACEMENT_3D('',#16358,#11790,#11791);
#9537=AXIS2_PLACEMENT_3D('',#16359,#11792,#11793);
#9538=AXIS2_PLACEMENT_3D('',#16360,#11794,#11795);
#9539=AXIS2_PLACEMENT_3D('',#16361,#11796,#11797);
#9540=AXIS2_PLACEMENT_3D('',#16362,#11798,#11799);
#9541=AXIS2_PLACEMENT_3D('',#16364,#11800,#11801);
#9542=AXIS2_PLACEMENT_3D('',#16365,#11802,#11803);
#9543=AXIS2_PLACEMENT_3D('',#16367,#11804,#11805);
#9544=AXIS2_PLACEMENT_3D('',#16369,#11807,#11808);
#9545=AXIS2_PLACEMENT_3D('',#16371,#11809,#11810);
#9546=AXIS2_PLACEMENT_3D('',#16373,#11812,#11813);
#9547=AXIS2_PLACEMENT_3D('',#16375,#11814,#11815);
#9548=AXIS2_PLACEMENT_3D('',#16377,#11817,#11818);
#9549=AXIS2_PLACEMENT_3D('',#16379,#11819,#11820);
#9550=AXIS2_PLACEMENT_3D('',#16380,#11821,#11822);
#9551=AXIS2_PLACEMENT_3D('',#16382,#11823,#11824);
#9552=AXIS2_PLACEMENT_3D('',#16384,#11826,#11827);
#9553=AXIS2_PLACEMENT_3D('',#16386,#11828,#11829);
#9554=AXIS2_PLACEMENT_3D('',#16388,#11831,#11832);
#9555=AXIS2_PLACEMENT_3D('',#16390,#11833,#11834);
#9556=AXIS2_PLACEMENT_3D('',#16392,#11836,#11837);
#9557=AXIS2_PLACEMENT_3D('',#16393,#11838,#11839);
#9558=AXIS2_PLACEMENT_3D('',#16402,#11844,#11845);
#9559=AXIS2_PLACEMENT_3D('',#16408,#11849,#11850);
#9560=AXIS2_PLACEMENT_3D('',#16414,#11854,#11855);
#9561=AXIS2_PLACEMENT_3D('',#16420,#11859,#11860);
#9562=AXIS2_PLACEMENT_3D('',#16426,#11864,#11865);
#9563=AXIS2_PLACEMENT_3D('',#16429,#11868,#11869);
#9564=AXIS2_PLACEMENT_3D('',#16430,#11870,#11871);
#9565=AXIS2_PLACEMENT_3D('',#16431,#11872,#11873);
#9566=AXIS2_PLACEMENT_3D('',#16432,#11874,#11875);
#9567=AXIS2_PLACEMENT_3D('',#16433,#11876,#11877);
#9568=AXIS2_PLACEMENT_3D('',#16434,#11878,#11879);
#9569=AXIS2_PLACEMENT_3D('',#16435,#11880,#11881);
#9570=AXIS2_PLACEMENT_3D('',#16436,#11882,#11883);
#9571=AXIS2_PLACEMENT_3D('',#16437,#11884,#11885);
#9572=AXIS2_PLACEMENT_3D('',#16438,#11886,#11887);
#9573=AXIS2_PLACEMENT_3D('',#16439,#11888,#11889);
#9574=AXIS2_PLACEMENT_3D('',#16440,#11890,#11891);
#9575=AXIS2_PLACEMENT_3D('',#16441,#11892,#11893);
#9576=AXIS2_PLACEMENT_3D('',#16442,#11894,#11895);
#9577=AXIS2_PLACEMENT_3D('',#16443,#11896,#11897);
#9578=AXIS2_PLACEMENT_3D('',#16444,#11898,#11899);
#9579=AXIS2_PLACEMENT_3D('',#16445,#11900,#11901);
#9580=AXIS2_PLACEMENT_3D('',#16446,#11902,#11903);
#9581=AXIS2_PLACEMENT_3D('',#16447,#11904,#11905);
#9582=AXIS2_PLACEMENT_3D('',#16448,#11906,#11907);
#9583=AXIS2_PLACEMENT_3D('',#16449,#11908,#11909);
#9584=AXIS2_PLACEMENT_3D('',#16450,#11910,#11911);
#9585=AXIS2_PLACEMENT_3D('',#16451,#11912,#11913);
#9586=AXIS2_PLACEMENT_3D('',#16452,#11914,#11915);
#9587=AXIS2_PLACEMENT_3D('',#16453,#11916,#11917);
#9588=AXIS2_PLACEMENT_3D('',#16454,#11918,#11919);
#9589=AXIS2_PLACEMENT_3D('',#16455,#11920,#11921);
#9590=AXIS2_PLACEMENT_3D('',#16456,#11922,#11923);
#9591=AXIS2_PLACEMENT_3D('',#16457,#11924,#11925);
#9592=AXIS2_PLACEMENT_3D('',#16458,#11926,#11927);
#9593=AXIS2_PLACEMENT_3D('',#16459,#11928,#11929);
#9594=AXIS2_PLACEMENT_3D('',#16460,#11930,#11931);
#9595=AXIS2_PLACEMENT_3D('',#16461,#11932,#11933);
#9596=AXIS2_PLACEMENT_3D('',#16462,#11934,#11935);
#9597=AXIS2_PLACEMENT_3D('',#16463,#11936,#11937);
#9598=AXIS2_PLACEMENT_3D('',#16464,#11938,#11939);
#9599=AXIS2_PLACEMENT_3D('',#16465,#11940,#11941);
#9600=AXIS2_PLACEMENT_3D('',#16466,#11942,#11943);
#9601=AXIS2_PLACEMENT_3D('',#16467,#11944,#11945);
#9602=AXIS2_PLACEMENT_3D('',#16468,#11946,#11947);
#9603=AXIS2_PLACEMENT_3D('',#16469,#11948,#11949);
#9604=AXIS2_PLACEMENT_3D('',#16470,#11950,#11951);
#9605=AXIS2_PLACEMENT_3D('',#16471,#11952,#11953);
#9606=AXIS2_PLACEMENT_3D('',#16472,#11954,#11955);
#9607=AXIS2_PLACEMENT_3D('',#16473,#11956,#11957);
#9608=AXIS2_PLACEMENT_3D('',#16474,#11958,#11959);
#9609=AXIS2_PLACEMENT_3D('',#16475,#11960,#11961);
#9610=AXIS2_PLACEMENT_3D('',#16476,#11962,#11963);
#9611=AXIS2_PLACEMENT_3D('',#16477,#11964,#11965);
#9612=AXIS2_PLACEMENT_3D('',#16478,#11966,#11967);
#9613=AXIS2_PLACEMENT_3D('',#16479,#11968,#11969);
#9614=AXIS2_PLACEMENT_3D('',#16480,#11970,#11971);
#9615=AXIS2_PLACEMENT_3D('',#16481,#11972,#11973);
#9616=AXIS2_PLACEMENT_3D('',#16482,#11974,#11975);
#9617=AXIS2_PLACEMENT_3D('',#16483,#11976,#11977);
#9618=AXIS2_PLACEMENT_3D('',#16484,#11978,#11979);
#9619=AXIS2_PLACEMENT_3D('',#16485,#11980,#11981);
#9620=AXIS2_PLACEMENT_3D('',#16486,#11982,#11983);
#9621=AXIS2_PLACEMENT_3D('',#16487,#11984,#11985);
#9622=AXIS2_PLACEMENT_3D('',#16488,#11986,#11987);
#9623=AXIS2_PLACEMENT_3D('',#16489,#11988,#11989);
#9624=AXIS2_PLACEMENT_3D('',#16490,#11990,#11991);
#9625=AXIS2_PLACEMENT_3D('',#16491,#11992,#11993);
#9626=AXIS2_PLACEMENT_3D('',#16492,#11994,#11995);
#9627=AXIS2_PLACEMENT_3D('',#16493,#11996,#11997);
#9628=AXIS2_PLACEMENT_3D('',#16494,#11998,#11999);
#9629=AXIS2_PLACEMENT_3D('',#16495,#12000,#12001);
#9630=AXIS2_PLACEMENT_3D('',#16496,#12002,#12003);
#9631=AXIS2_PLACEMENT_3D('',#16497,#12004,#12005);
#9632=AXIS2_PLACEMENT_3D('',#16498,#12006,#12007);
#9633=AXIS2_PLACEMENT_3D('',#16499,#12008,#12009);
#9634=AXIS2_PLACEMENT_3D('',#16500,#12010,#12011);
#9635=AXIS2_PLACEMENT_3D('',#16501,#12012,#12013);
#9636=AXIS2_PLACEMENT_3D('',#16502,#12014,#12015);
#9637=AXIS2_PLACEMENT_3D('',#16503,#12016,#12017);
#9638=AXIS2_PLACEMENT_3D('',#16504,#12018,#12019);
#9639=AXIS2_PLACEMENT_3D('',#16505,#12020,#12021);
#9640=AXIS2_PLACEMENT_3D('',#16506,#12022,#12023);
#9641=AXIS2_PLACEMENT_3D('',#16507,#12024,#12025);
#9642=AXIS2_PLACEMENT_3D('',#16508,#12026,#12027);
#9643=AXIS2_PLACEMENT_3D('',#16509,#12028,#12029);
#9644=AXIS2_PLACEMENT_3D('',#16510,#12030,#12031);
#9645=AXIS2_PLACEMENT_3D('',#16519,#12036,#12037);
#9646=AXIS2_PLACEMENT_3D('',#16521,#12038,#12039);
#9647=AXIS2_PLACEMENT_3D('',#16525,#12042,#12043);
#9648=AXIS2_PLACEMENT_3D('',#16529,#12046,#12047);
#9649=AXIS2_PLACEMENT_3D('',#16533,#12050,#12051);
#9650=AXIS2_PLACEMENT_3D('',#16534,#12052,#12053);
#9651=AXIS2_PLACEMENT_3D('',#16535,#12054,#12055);
#9652=AXIS2_PLACEMENT_3D('',#16537,#12056,#12057);
#9653=AXIS2_PLACEMENT_3D('',#16539,#12058,#12059);
#9654=AXIS2_PLACEMENT_3D('',#16540,#12060,#12061);
#9655=AXIS2_PLACEMENT_3D('',#16542,#12062,#12063);
#9656=AXIS2_PLACEMENT_3D('',#16544,#12064,#12065);
#9657=AXIS2_PLACEMENT_3D('',#16545,#12066,#12067);
#9658=AXIS2_PLACEMENT_3D('',#16547,#12069,#12070);
#9659=AXIS2_PLACEMENT_3D('',#16550,#12072,#12073);
#9660=AXIS2_PLACEMENT_3D('',#16551,#12074,#12075);
#9661=AXIS2_PLACEMENT_3D('',#16553,#12076,#12077);
#9662=AXIS2_PLACEMENT_3D('',#16555,#12079,#12080);
#9663=AXIS2_PLACEMENT_3D('',#16556,#12081,#12082);
#9664=AXIS2_PLACEMENT_3D('',#16557,#12083,#12084);
#9665=AXIS2_PLACEMENT_3D('',#16558,#12085,#12086);
#9666=AXIS2_PLACEMENT_3D('',#16567,#12091,#12092);
#9667=AXIS2_PLACEMENT_3D('',#16573,#12096,#12097);
#9668=AXIS2_PLACEMENT_3D('',#16579,#12101,#12102);
#9669=AXIS2_PLACEMENT_3D('',#16581,#12103,#12104);
#9670=AXIS2_PLACEMENT_3D('',#16582,#12105,#12106);
#9671=AXIS2_PLACEMENT_3D('',#16583,#12107,#12108);
#9672=AXIS2_PLACEMENT_3D('',#16584,#12109,#12110);
#9673=AXIS2_PLACEMENT_3D('',#16585,#12111,#12112);
#9674=AXIS2_PLACEMENT_3D('',#16587,#12113,#12114);
#9675=AXIS2_PLACEMENT_3D('',#16589,#12115,#12116);
#9676=AXIS2_PLACEMENT_3D('',#16590,#12117,#12118);
#9677=AXIS2_PLACEMENT_3D('',#16593,#12120,#12121);
#9678=AXIS2_PLACEMENT_3D('',#16594,#12122,#12123);
#9679=AXIS2_PLACEMENT_3D('',#16596,#12125,#12126);
#9680=AXIS2_PLACEMENT_3D('',#16597,#12127,#12128);
#9681=AXIS2_PLACEMENT_3D('',#16598,#12129,#12130);
#9682=AXIS2_PLACEMENT_3D('',#16600,#12131,#12132);
#9683=AXIS2_PLACEMENT_3D('',#16603,#12134,#12135);
#9684=AXIS2_PLACEMENT_3D('',#16604,#12136,#12137);
#9685=AXIS2_PLACEMENT_3D('',#16606,#12138,#12139);
#9686=AXIS2_PLACEMENT_3D('',#16609,#12141,#12142);
#9687=AXIS2_PLACEMENT_3D('',#16610,#12143,#12144);
#9688=AXIS2_PLACEMENT_3D('',#16611,#12145,#12146);
#9689=AXIS2_PLACEMENT_3D('',#16612,#12147,#12148);
#9690=AXIS2_PLACEMENT_3D('',#16613,#12149,#12150);
#9691=AXIS2_PLACEMENT_3D('',#16615,#12151,#12152);
#9692=AXIS2_PLACEMENT_3D('',#16618,#12154,#12155);
#9693=AXIS2_PLACEMENT_3D('',#16619,#12156,#12157);
#9694=AXIS2_PLACEMENT_3D('',#16621,#12158,#12159);
#9695=AXIS2_PLACEMENT_3D('',#16624,#12161,#12162);
#9696=AXIS2_PLACEMENT_3D('',#16625,#12163,#12164);
#9697=AXIS2_PLACEMENT_3D('',#16626,#12165,#12166);
#9698=AXIS2_PLACEMENT_3D('',#16627,#12167,#12168);
#9699=AXIS2_PLACEMENT_3D('',#16628,#12169,#12170);
#9700=AXIS2_PLACEMENT_3D('',#16632,#12172,#12173);
#9701=AXIS2_PLACEMENT_3D('',#16633,#12174,#12175);
#9702=AXIS2_PLACEMENT_3D('',#16643,#12176,#12177);
#9703=AXIS2_PLACEMENT_3D('',#16705,#12179,#12180);
#9704=AXIS2_PLACEMENT_3D('',#16707,#12182,#12183);
#9705=AXIS2_PLACEMENT_3D('',#16709,#12184,#12185);
#9706=AXIS2_PLACEMENT_3D('',#16713,#12188,#12189);
#9707=AXIS2_PLACEMENT_3D('',#16714,#12190,#12191);
#9708=AXIS2_PLACEMENT_3D('',#16716,#12192,#12193);
#9709=AXIS2_PLACEMENT_3D('',#16720,#12196,#12197);
#9710=AXIS2_PLACEMENT_3D('',#16721,#12198,#12199);
#9711=AXIS2_PLACEMENT_3D('',#16722,#12200,#12201);
#9712=AXIS2_PLACEMENT_3D('',#16723,#12202,#12203);
#9713=AXIS2_PLACEMENT_3D('',#16724,#12204,#12205);
#9714=AXIS2_PLACEMENT_3D('',#16728,#12207,#12208);
#9715=AXIS2_PLACEMENT_3D('',#16729,#12209,#12210);
#9716=AXIS2_PLACEMENT_3D('',#16739,#12211,#12212);
#9717=AXIS2_PLACEMENT_3D('',#16801,#12214,#12215);
#9718=AXIS2_PLACEMENT_3D('',#16803,#12217,#12218);
#9719=AXIS2_PLACEMENT_3D('',#16805,#12219,#12220);
#9720=AXIS2_PLACEMENT_3D('',#16809,#12223,#12224);
#9721=AXIS2_PLACEMENT_3D('',#16810,#12225,#12226);
#9722=AXIS2_PLACEMENT_3D('',#16812,#12227,#12228);
#9723=AXIS2_PLACEMENT_3D('',#16816,#12231,#12232);
#9724=AXIS2_PLACEMENT_3D('',#16817,#12233,#12234);
#9725=AXIS2_PLACEMENT_3D('',#16818,#12235,#12236);
#9726=AXIS2_PLACEMENT_3D('',#16819,#12237,#12238);
#9727=AXIS2_PLACEMENT_3D('',#16820,#12239,#12240);
#9728=AXIS2_PLACEMENT_3D('',#16837,#12249,#12250);
#9729=AXIS2_PLACEMENT_3D('',#16843,#12254,#12255);
#9730=AXIS2_PLACEMENT_3D('',#16847,#12258,#12259);
#9731=AXIS2_PLACEMENT_3D('',#16851,#12262,#12263);
#9732=AXIS2_PLACEMENT_3D('',#16855,#12266,#12267);
#9733=AXIS2_PLACEMENT_3D('',#16863,#12272,#12273);
#9734=AXIS2_PLACEMENT_3D('',#16865,#12275,#12276);
#9735=AXIS2_PLACEMENT_3D('',#16867,#12278,#12279);
#9736=AXIS2_PLACEMENT_3D('',#16869,#12281,#12282);
#9737=AXIS2_PLACEMENT_3D('',#16870,#12283,#12284);
#9738=AXIS2_PLACEMENT_3D('',#16871,#12285,#12286);
#9739=AXIS2_PLACEMENT_3D('',#16873,#12287,#12288);
#9740=AXIS2_PLACEMENT_3D('',#16874,#12289,#12290);
#9741=AXIS2_PLACEMENT_3D('',#16883,#12295,#12296);
#9742=AXIS2_PLACEMENT_3D('',#16889,#12300,#12301);
#9743=AXIS2_PLACEMENT_3D('',#16895,#12305,#12306);
#9744=AXIS2_PLACEMENT_3D('',#16901,#12310,#12311);
#9745=AXIS2_PLACEMENT_3D('',#16907,#12315,#12316);
#9746=AXIS2_PLACEMENT_3D('',#16910,#12319,#12320);
#9747=AXIS2_PLACEMENT_3D('',#16911,#12321,#12322);
#9748=AXIS2_PLACEMENT_3D('',#16913,#12323,#12324);
#9749=AXIS2_PLACEMENT_3D('',#16914,#12325,#12326);
#9750=AXIS2_PLACEMENT_3D('',#16916,#12327,#12328);
#9751=AXIS2_PLACEMENT_3D('',#16918,#12330,#12331);
#9752=AXIS2_PLACEMENT_3D('',#16920,#12333,#12334);
#9753=AXIS2_PLACEMENT_3D('',#16921,#12335,#12336);
#9754=AXIS2_PLACEMENT_3D('',#16922,#12337,#12338);
#9755=AXIS2_PLACEMENT_3D('',#16923,#12339,#12340);
#9756=AXIS2_PLACEMENT_3D('',#16924,#12341,#12342);
#9757=AXIS2_PLACEMENT_3D('',#16925,#12343,#12344);
#9758=AXIS2_PLACEMENT_3D('',#16926,#12345,#12346);
#9759=AXIS2_PLACEMENT_3D('',#16927,#12347,#12348);
#9760=AXIS2_PLACEMENT_3D('',#16928,#12349,#12350);
#9761=AXIS2_PLACEMENT_3D('',#16929,#12351,#12352);
#9762=AXIS2_PLACEMENT_3D('',#16930,#12353,#12354);
#9763=AXIS2_PLACEMENT_3D('',#16931,#12355,#12356);
#9764=AXIS2_PLACEMENT_3D('',#16932,#12357,#12358);
#9765=AXIS2_PLACEMENT_3D('',#16933,#12359,#12360);
#9766=AXIS2_PLACEMENT_3D('',#16934,#12361,#12362);
#9767=AXIS2_PLACEMENT_3D('',#16935,#12363,#12364);
#9768=AXIS2_PLACEMENT_3D('',#16936,#12365,#12366);
#9769=AXIS2_PLACEMENT_3D('',#16937,#12367,#12368);
#9770=AXIS2_PLACEMENT_3D('',#16938,#12369,#12370);
#9771=AXIS2_PLACEMENT_3D('',#16939,#12371,#12372);
#9772=AXIS2_PLACEMENT_3D('',#16940,#12373,#12374);
#9773=DIRECTION('axis',(0.,0.,1.));
#9774=DIRECTION('refdir',(1.,0.,0.));
#9775=DIRECTION('axis',(0.,0.,1.));
#9776=DIRECTION('refdir',(1.,0.,0.));
#9777=DIRECTION('axis',(0.,0.,1.));
#9778=DIRECTION('refdir',(1.,0.,0.));
#9779=DIRECTION('center_axis',(0.,0.,1.));
#9780=DIRECTION('ref_axis',(1.,0.,0.));
#9781=DIRECTION('center_axis',(0.,0.,1.));
#9782=DIRECTION('ref_axis',(1.,0.,0.));
#9783=DIRECTION('',(0.,0.,1.));
#9784=DIRECTION('center_axis',(0.,0.,-1.));
#9785=DIRECTION('ref_axis',(1.,0.,0.));
#9786=DIRECTION('center_axis',(0.,0.,1.));
#9787=DIRECTION('ref_axis',(1.,0.,0.));
#9788=DIRECTION('center_axis',(0.,0.,1.));
#9789=DIRECTION('ref_axis',(1.,0.,0.));
#9790=DIRECTION('',(0.,0.,1.));
#9791=DIRECTION('center_axis',(0.,0.,-1.));
#9792=DIRECTION('ref_axis',(1.,0.,0.));
#9793=DIRECTION('center_axis',(0.,0.,1.));
#9794=DIRECTION('ref_axis',(1.,0.,0.));
#9795=DIRECTION('center_axis',(0.,0.,1.));
#9796=DIRECTION('ref_axis',(1.,0.,0.));
#9797=DIRECTION('',(0.,0.,1.));
#9798=DIRECTION('center_axis',(0.,0.,-1.));
#9799=DIRECTION('ref_axis',(1.,0.,0.));
#9800=DIRECTION('center_axis',(0.,0.,1.));
#9801=DIRECTION('ref_axis',(1.,0.,0.));
#9802=DIRECTION('center_axis',(0.,0.,1.));
#9803=DIRECTION('ref_axis',(1.,0.,0.));
#9804=DIRECTION('',(0.,0.,1.));
#9805=DIRECTION('center_axis',(0.,0.,-1.));
#9806=DIRECTION('ref_axis',(1.,0.,0.));
#9807=DIRECTION('center_axis',(0.,0.,1.));
#9808=DIRECTION('ref_axis',(1.,0.,0.));
#9809=DIRECTION('center_axis',(0.,0.,1.));
#9810=DIRECTION('ref_axis',(1.,0.,0.));
#9811=DIRECTION('',(0.,0.,1.));
#9812=DIRECTION('center_axis',(0.,0.,-1.));
#9813=DIRECTION('ref_axis',(1.,0.,0.));
#9814=DIRECTION('center_axis',(0.,0.,1.));
#9815=DIRECTION('ref_axis',(1.,0.,0.));
#9816=DIRECTION('center_axis',(0.,0.,1.));
#9817=DIRECTION('ref_axis',(1.,0.,0.));
#9818=DIRECTION('',(0.,0.,1.));
#9819=DIRECTION('center_axis',(0.,0.,-1.));
#9820=DIRECTION('ref_axis',(1.,0.,0.));
#9821=DIRECTION('center_axis',(0.,0.,1.));
#9822=DIRECTION('ref_axis',(1.,0.,0.));
#9823=DIRECTION('center_axis',(0.,0.,1.));
#9824=DIRECTION('ref_axis',(1.,0.,0.));
#9825=DIRECTION('',(0.,0.,1.));
#9826=DIRECTION('center_axis',(0.,0.,-1.));
#9827=DIRECTION('ref_axis',(1.,0.,0.));
#9828=DIRECTION('center_axis',(0.,0.,1.));
#9829=DIRECTION('ref_axis',(1.,0.,0.));
#9830=DIRECTION('center_axis',(0.,0.,1.));
#9831=DIRECTION('ref_axis',(1.,0.,0.));
#9832=DIRECTION('',(0.,0.,1.));
#9833=DIRECTION('center_axis',(0.,0.,-1.));
#9834=DIRECTION('ref_axis',(1.,0.,0.));
#9835=DIRECTION('center_axis',(0.,0.,1.));
#9836=DIRECTION('ref_axis',(1.,0.,0.));
#9837=DIRECTION('center_axis',(0.,0.,1.));
#9838=DIRECTION('ref_axis',(1.,0.,0.));
#9839=DIRECTION('',(0.,0.,1.));
#9840=DIRECTION('center_axis',(0.,0.,-1.));
#9841=DIRECTION('ref_axis',(1.,0.,0.));
#9842=DIRECTION('center_axis',(0.,0.,1.));
#9843=DIRECTION('ref_axis',(1.,0.,0.));
#9844=DIRECTION('center_axis',(0.,0.,1.));
#9845=DIRECTION('ref_axis',(1.,0.,0.));
#9846=DIRECTION('',(0.,0.,1.));
#9847=DIRECTION('center_axis',(0.,0.,-1.));
#9848=DIRECTION('ref_axis',(1.,0.,0.));
#9849=DIRECTION('center_axis',(0.,1.,0.));
#9850=DIRECTION('ref_axis',(-1.,0.,0.));
#9851=DIRECTION('',(-1.,0.,0.));
#9852=DIRECTION('',(0.,0.,1.));
#9853=DIRECTION('',(-1.,0.,0.));
#9854=DIRECTION('',(0.,0.,1.));
#9855=DIRECTION('center_axis',(1.,0.,0.));
#9856=DIRECTION('ref_axis',(0.,1.,0.));
#9857=DIRECTION('',(0.,1.,0.));
#9858=DIRECTION('',(0.,1.,0.));
#9859=DIRECTION('',(0.,0.,1.));
#9860=DIRECTION('center_axis',(0.,-1.,0.));
#9861=DIRECTION('ref_axis',(1.,0.,0.));
#9862=DIRECTION('',(1.,0.,0.));
#9863=DIRECTION('',(1.,0.,0.));
#9864=DIRECTION('',(0.,0.,1.));
#9865=DIRECTION('center_axis',(-1.,0.,0.));
#9866=DIRECTION('ref_axis',(0.,-1.,0.));
#9867=DIRECTION('',(0.,-1.,0.));
#9868=DIRECTION('',(0.,-1.,0.));
#9869=DIRECTION('center_axis',(0.,0.,1.));
#9870=DIRECTION('ref_axis',(1.,0.,0.));
#9871=DIRECTION('center_axis',(0.,0.,1.));
#9872=DIRECTION('ref_axis',(1.,0.,0.));
#9873=DIRECTION('axis',(0.,0.,1.));
#9874=DIRECTION('refdir',(1.,0.,0.));
#9875=DIRECTION('center_axis',(0.,1.,0.));
#9876=DIRECTION('ref_axis',(-1.,0.,0.));
#9877=DIRECTION('',(-1.,0.,0.));
#9878=DIRECTION('',(0.,0.,1.));
#9879=DIRECTION('',(-1.,0.,0.));
#9880=DIRECTION('',(0.,0.,1.));
#9881=DIRECTION('center_axis',(1.,0.,0.));
#9882=DIRECTION('ref_axis',(0.,1.,0.));
#9883=DIRECTION('',(0.,1.,0.));
#9884=DIRECTION('',(0.,1.,0.));
#9885=DIRECTION('',(0.,0.,1.));
#9886=DIRECTION('center_axis',(0.,-1.,0.));
#9887=DIRECTION('ref_axis',(1.,0.,0.));
#9888=DIRECTION('',(1.,0.,0.));
#9889=DIRECTION('',(1.,0.,0.));
#9890=DIRECTION('',(0.,0.,1.));
#9891=DIRECTION('center_axis',(-1.,0.,0.));
#9892=DIRECTION('ref_axis',(0.,-1.,0.));
#9893=DIRECTION('',(0.,-1.,0.));
#9894=DIRECTION('',(0.,-1.,0.));
#9895=DIRECTION('center_axis',(0.,0.,1.));
#9896=DIRECTION('ref_axis',(1.,0.,0.));
#9897=DIRECTION('center_axis',(0.,0.,1.));
#9898=DIRECTION('ref_axis',(1.,0.,0.));
#9899=DIRECTION('axis',(0.,0.,1.));
#9900=DIRECTION('refdir',(1.,0.,0.));
#9901=DIRECTION('center_axis',(0.,1.,0.));
#9902=DIRECTION('ref_axis',(-1.,0.,0.));
#9903=DIRECTION('',(-1.,0.,0.));
#9904=DIRECTION('',(0.,0.,1.));
#9905=DIRECTION('',(-1.,0.,0.));
#9906=DIRECTION('',(0.,0.,1.));
#9907=DIRECTION('center_axis',(1.,0.,0.));
#9908=DIRECTION('ref_axis',(0.,1.,0.));
#9909=DIRECTION('',(0.,1.,0.));
#9910=DIRECTION('',(0.,1.,0.));
#9911=DIRECTION('',(0.,0.,1.));
#9912=DIRECTION('center_axis',(0.,-1.,0.));
#9913=DIRECTION('ref_axis',(1.,0.,0.));
#9914=DIRECTION('',(1.,0.,0.));
#9915=DIRECTION('',(1.,0.,0.));
#9916=DIRECTION('',(0.,0.,1.));
#9917=DIRECTION('center_axis',(-1.,0.,0.));
#9918=DIRECTION('ref_axis',(0.,-1.,0.));
#9919=DIRECTION('',(0.,-1.,0.));
#9920=DIRECTION('',(0.,-1.,0.));
#9921=DIRECTION('center_axis',(0.,0.,1.));
#9922=DIRECTION('ref_axis',(1.,0.,0.));
#9923=DIRECTION('center_axis',(0.,0.,1.));
#9924=DIRECTION('ref_axis',(1.,0.,0.));
#9925=DIRECTION('axis',(0.,0.,1.));
#9926=DIRECTION('refdir',(1.,0.,0.));
#9927=DIRECTION('center_axis',(0.,0.,1.));
#9928=DIRECTION('ref_axis',(1.,0.,0.));
#9929=DIRECTION('center_axis',(0.,0.,1.));
#9930=DIRECTION('ref_axis',(1.,0.,0.));
#9931=DIRECTION('',(0.,0.,1.));
#9932=DIRECTION('center_axis',(0.,0.,-1.));
#9933=DIRECTION('ref_axis',(1.,0.,0.));
#9934=DIRECTION('center_axis',(0.,0.,1.));
#9935=DIRECTION('ref_axis',(1.,0.,0.));
#9936=DIRECTION('center_axis',(0.,0.,1.));
#9937=DIRECTION('ref_axis',(1.,0.,0.));
#9938=DIRECTION('',(0.,0.,1.));
#9939=DIRECTION('center_axis',(0.,0.,-1.));
#9940=DIRECTION('ref_axis',(1.,0.,0.));
#9941=DIRECTION('center_axis',(0.,0.,1.));
#9942=DIRECTION('ref_axis',(1.,0.,0.));
#9943=DIRECTION('center_axis',(0.,0.,1.));
#9944=DIRECTION('ref_axis',(1.,0.,0.));
#9945=DIRECTION('',(0.,0.,1.));
#9946=DIRECTION('center_axis',(0.,0.,-1.));
#9947=DIRECTION('ref_axis',(1.,0.,0.));
#9948=DIRECTION('center_axis',(0.,0.,1.));
#9949=DIRECTION('ref_axis',(1.,0.,0.));
#9950=DIRECTION('center_axis',(0.,0.,1.));
#9951=DIRECTION('ref_axis',(1.,0.,0.));
#9952=DIRECTION('',(0.,0.,1.));
#9953=DIRECTION('center_axis',(0.,0.,-1.));
#9954=DIRECTION('ref_axis',(1.,0.,0.));
#9955=DIRECTION('center_axis',(0.,0.,1.));
#9956=DIRECTION('ref_axis',(1.,0.,0.));
#9957=DIRECTION('',(0.,0.,1.));
#9958=DIRECTION('center_axis',(0.,0.,-1.));
#9959=DIRECTION('ref_axis',(1.,0.,0.));
#9960=DIRECTION('',(0.,0.,1.));
#9961=DIRECTION('center_axis',(0.,0.,1.));
#9962=DIRECTION('ref_axis',(1.,0.,0.));
#9963=DIRECTION('center_axis',(0.,0.,1.));
#9964=DIRECTION('ref_axis',(1.,0.,0.));
#9965=DIRECTION('',(0.,0.,1.));
#9966=DIRECTION('center_axis',(0.,0.,-1.));
#9967=DIRECTION('ref_axis',(1.,0.,0.));
#9968=DIRECTION('',(0.,0.,1.));
#9969=DIRECTION('center_axis',(0.,0.,1.));
#9970=DIRECTION('ref_axis',(1.,0.,0.));
#9971=DIRECTION('center_axis',(0.,0.,1.));
#9972=DIRECTION('ref_axis',(1.,0.,0.));
#9973=DIRECTION('',(0.,-1.,0.));
#9974=DIRECTION('',(1.,0.,0.));
#9975=DIRECTION('',(0.,1.,0.));
#9976=DIRECTION('',(-1.,0.,0.));
#9977=DIRECTION('',(0.,1.,0.));
#9978=DIRECTION('',(0.,-1.,0.));
#9979=DIRECTION('center_axis',(0.,0.,-1.));
#9980=DIRECTION('ref_axis',(1.,0.,0.));
#9981=DIRECTION('',(0.,1.,0.));
#9982=DIRECTION('center_axis',(0.,0.,-1.));
#9983=DIRECTION('ref_axis',(1.,0.,0.));
#9984=DIRECTION('',(0.,-1.,0.));
#9985=DIRECTION('center_axis',(0.,0.,-1.));
#9986=DIRECTION('ref_axis',(1.,0.,0.));
#9987=DIRECTION('',(0.,1.,0.));
#9988=DIRECTION('center_axis',(0.,0.,-1.));
#9989=DIRECTION('ref_axis',(1.,0.,0.));
#9990=DIRECTION('',(0.,-1.,0.));
#9991=DIRECTION('center_axis',(0.,0.,-1.));
#9992=DIRECTION('ref_axis',(1.,0.,0.));
#9993=DIRECTION('',(0.,1.,0.));
#9994=DIRECTION('center_axis',(0.,0.,-1.));
#9995=DIRECTION('ref_axis',(1.,0.,0.));
#9996=DIRECTION('',(0.,-1.,0.));
#9997=DIRECTION('center_axis',(-1.,0.,0.));
#9998=DIRECTION('ref_axis',(0.,-1.,0.));
#9999=DIRECTION('',(0.,-1.,0.));
#10000=DIRECTION('center_axis',(1.,0.,0.));
#10001=DIRECTION('ref_axis',(0.,1.,0.));
#10002=DIRECTION('',(0.,1.,0.));
#10003=DIRECTION('center_axis',(0.,0.,1.));
#10004=DIRECTION('ref_axis',(1.,0.,0.));
#10005=DIRECTION('',(0.,0.,1.));
#10006=DIRECTION('',(0.,0.,1.));
#10007=DIRECTION('center_axis',(0.,0.,1.));
#10008=DIRECTION('ref_axis',(1.,0.,0.));
#10009=DIRECTION('center_axis',(0.,0.,1.));
#10010=DIRECTION('ref_axis',(1.,0.,0.));
#10011=DIRECTION('',(0.,0.,1.));
#10012=DIRECTION('',(0.,0.,1.));
#10013=DIRECTION('center_axis',(0.,0.,1.));
#10014=DIRECTION('ref_axis',(1.,0.,0.));
#10015=DIRECTION('center_axis',(-1.,0.,0.));
#10016=DIRECTION('ref_axis',(0.,-1.,0.));
#10017=DIRECTION('',(0.,-1.,0.));
#10018=DIRECTION('center_axis',(1.,0.,0.));
#10019=DIRECTION('ref_axis',(0.,1.,0.));
#10020=DIRECTION('',(0.,1.,0.));
#10021=DIRECTION('center_axis',(0.,0.,1.));
#10022=DIRECTION('ref_axis',(1.,0.,0.));
#10023=DIRECTION('',(0.,0.,1.));
#10024=DIRECTION('',(0.,0.,1.));
#10025=DIRECTION('center_axis',(0.,0.,1.));
#10026=DIRECTION('ref_axis',(1.,0.,0.));
#10027=DIRECTION('center_axis',(0.,0.,1.));
#10028=DIRECTION('ref_axis',(1.,0.,0.));
#10029=DIRECTION('',(0.,0.,1.));
#10030=DIRECTION('',(0.,0.,1.));
#10031=DIRECTION('center_axis',(0.,0.,1.));
#10032=DIRECTION('ref_axis',(1.,0.,0.));
#10033=DIRECTION('center_axis',(-1.,0.,0.));
#10034=DIRECTION('ref_axis',(0.,-1.,0.));
#10035=DIRECTION('',(0.,-1.,0.));
#10036=DIRECTION('center_axis',(1.,0.,0.));
#10037=DIRECTION('ref_axis',(0.,1.,0.));
#10038=DIRECTION('',(0.,1.,0.));
#10039=DIRECTION('center_axis',(0.,0.,1.));
#10040=DIRECTION('ref_axis',(1.,0.,0.));
#10041=DIRECTION('',(0.,0.,1.));
#10042=DIRECTION('',(0.,0.,1.));
#10043=DIRECTION('center_axis',(0.,0.,1.));
#10044=DIRECTION('ref_axis',(1.,0.,0.));
#10045=DIRECTION('center_axis',(0.,0.,1.));
#10046=DIRECTION('ref_axis',(1.,0.,0.));
#10047=DIRECTION('',(0.,0.,1.));
#10048=DIRECTION('',(0.,0.,1.));
#10049=DIRECTION('center_axis',(0.,0.,1.));
#10050=DIRECTION('ref_axis',(1.,0.,0.));
#10051=DIRECTION('center_axis',(-1.,0.,0.));
#10052=DIRECTION('ref_axis',(0.,-1.,0.));
#10053=DIRECTION('',(0.,-1.,0.));
#10054=DIRECTION('center_axis',(1.,0.,0.));
#10055=DIRECTION('ref_axis',(0.,1.,0.));
#10056=DIRECTION('',(0.,1.,0.));
#10057=DIRECTION('center_axis',(0.,1.,0.));
#10058=DIRECTION('ref_axis',(-1.,0.,0.));
#10059=DIRECTION('',(-1.,0.,0.));
#10060=DIRECTION('',(0.,0.,1.));
#10061=DIRECTION('',(0.,0.,1.));
#10062=DIRECTION('center_axis',(1.,0.,0.));
#10063=DIRECTION('ref_axis',(0.,1.,0.));
#10064=DIRECTION('',(0.,1.,0.));
#10065=DIRECTION('',(0.,0.,1.));
#10066=DIRECTION('center_axis',(0.,-1.,0.));
#10067=DIRECTION('ref_axis',(1.,0.,0.));
#10068=DIRECTION('',(1.,0.,0.));
#10069=DIRECTION('',(0.,0.,1.));
#10070=DIRECTION('center_axis',(-1.,0.,0.));
#10071=DIRECTION('ref_axis',(0.,-1.,0.));
#10072=DIRECTION('',(0.,-1.,0.));
#10073=DIRECTION('center_axis',(0.,0.,1.));
#10074=DIRECTION('ref_axis',(1.,0.,0.));
#10075=DIRECTION('axis',(0.,0.,1.));
#10076=DIRECTION('refdir',(1.,0.,0.));
#10077=DIRECTION('center_axis',(0.,1.,0.));
#10078=DIRECTION('ref_axis',(1.,0.,0.));
#10079=DIRECTION('center_axis',(0.,1.,0.));
#10080=DIRECTION('ref_axis',(1.,0.,0.));
#10081=DIRECTION('',(0.,1.,0.));
#10082=DIRECTION('center_axis',(0.,-1.,0.));
#10083=DIRECTION('ref_axis',(1.,0.,0.));
#10084=DIRECTION('center_axis',(0.,1.,0.));
#10085=DIRECTION('ref_axis',(1.,0.,0.));
#10086=DIRECTION('center_axis',(0.,1.,0.));
#10087=DIRECTION('ref_axis',(1.,0.,0.));
#10088=DIRECTION('',(0.,1.,0.));
#10089=DIRECTION('center_axis',(0.,-1.,0.));
#10090=DIRECTION('ref_axis',(1.,0.,0.));
#10091=DIRECTION('center_axis',(0.,1.,0.));
#10092=DIRECTION('ref_axis',(1.,0.,0.));
#10093=DIRECTION('center_axis',(0.,1.,0.));
#10094=DIRECTION('ref_axis',(1.,0.,0.));
#10095=DIRECTION('',(0.,1.,0.));
#10096=DIRECTION('center_axis',(0.,-1.,0.));
#10097=DIRECTION('ref_axis',(1.,0.,0.));
#10098=DIRECTION('center_axis',(0.,1.,0.));
#10099=DIRECTION('ref_axis',(1.,0.,0.));
#10100=DIRECTION('center_axis',(0.,1.,0.));
#10101=DIRECTION('ref_axis',(1.,0.,0.));
#10102=DIRECTION('',(0.,1.,0.));
#10103=DIRECTION('center_axis',(0.,-1.,0.));
#10104=DIRECTION('ref_axis',(1.,0.,0.));
#10105=DIRECTION('center_axis',(0.,1.,0.));
#10106=DIRECTION('ref_axis',(1.,0.,0.));
#10107=DIRECTION('center_axis',(0.,1.,0.));
#10108=DIRECTION('ref_axis',(1.,0.,0.));
#10109=DIRECTION('',(0.,1.,0.));
#10110=DIRECTION('center_axis',(0.,-1.,0.));
#10111=DIRECTION('ref_axis',(1.,0.,0.));
#10112=DIRECTION('center_axis',(0.,0.,1.));
#10113=DIRECTION('ref_axis',(1.,0.,0.));
#10114=DIRECTION('center_axis',(0.,0.,1.));
#10115=DIRECTION('ref_axis',(1.,0.,0.));
#10116=DIRECTION('',(0.,0.,1.));
#10117=DIRECTION('center_axis',(0.,0.,-1.));
#10118=DIRECTION('ref_axis',(1.,0.,0.));
#10119=DIRECTION('center_axis',(0.,0.,1.));
#10120=DIRECTION('ref_axis',(1.,0.,0.));
#10121=DIRECTION('center_axis',(0.,0.,1.));
#10122=DIRECTION('ref_axis',(1.,0.,0.));
#10123=DIRECTION('',(0.,0.,1.));
#10124=DIRECTION('center_axis',(0.,0.,-1.));
#10125=DIRECTION('ref_axis',(1.,0.,0.));
#10126=DIRECTION('center_axis',(0.,0.,1.));
#10127=DIRECTION('ref_axis',(1.,0.,0.));
#10128=DIRECTION('',(0.,1.,0.));
#10129=DIRECTION('',(-1.,0.,0.));
#10130=DIRECTION('',(0.,1.,0.));
#10131=DIRECTION('',(1.,0.,0.));
#10132=DIRECTION('center_axis',(0.,0.,1.));
#10133=DIRECTION('ref_axis',(1.,0.,0.));
#10134=DIRECTION('',(0.,-1.,0.));
#10135=DIRECTION('',(1.,0.,0.));
#10136=DIRECTION('',(0.,1.,0.));
#10137=DIRECTION('',(-1.,0.,0.));
#10138=DIRECTION('center_axis',(-1.,0.,0.));
#10139=DIRECTION('ref_axis',(0.,0.,1.));
#10140=DIRECTION('',(0.,0.,-1.));
#10141=DIRECTION('',(0.,0.,1.));
#10142=DIRECTION('',(0.,1.,0.));
#10143=DIRECTION('center_axis',(1.,0.,0.));
#10144=DIRECTION('ref_axis',(0.,0.,-1.));
#10145=DIRECTION('',(0.,0.,1.));
#10146=DIRECTION('',(0.,1.,0.));
#10147=DIRECTION('',(0.,0.,-1.));
#10148=DIRECTION('center_axis',(0.,-1.,0.));
#10149=DIRECTION('ref_axis',(1.,0.,0.));
#10150=DIRECTION('',(0.,0.,1.));
#10151=DIRECTION('',(1.,0.,0.));
#10152=DIRECTION('',(0.,0.,1.));
#10153=DIRECTION('',(1.,0.,0.));
#10154=DIRECTION('center_axis',(1.,0.,0.));
#10155=DIRECTION('ref_axis',(0.,1.,0.));
#10156=DIRECTION('',(0.,0.,1.));
#10157=DIRECTION('',(0.,1.,0.));
#10158=DIRECTION('center_axis',(0.,1.,0.));
#10159=DIRECTION('ref_axis',(-1.,0.,0.));
#10160=DIRECTION('',(0.,0.,1.));
#10161=DIRECTION('',(-1.,0.,0.));
#10162=DIRECTION('',(-1.,0.,0.));
#10163=DIRECTION('center_axis',(-1.,0.,0.));
#10164=DIRECTION('ref_axis',(0.,-1.,0.));
#10165=DIRECTION('',(0.,-1.,0.));
#10166=DIRECTION('center_axis',(0.,0.,1.));
#10167=DIRECTION('ref_axis',(1.,0.,0.));
#10168=DIRECTION('center_axis',(0.,0.,1.));
#10169=DIRECTION('ref_axis',(1.,0.,0.));
#10170=DIRECTION('axis',(0.,0.,1.));
#10171=DIRECTION('refdir',(1.,0.,0.));
#10172=DIRECTION('center_axis',(0.,1.,0.));
#10173=DIRECTION('ref_axis',(1.,0.,0.));
#10174=DIRECTION('center_axis',(0.,1.,0.));
#10175=DIRECTION('ref_axis',(1.,0.,0.));
#10176=DIRECTION('',(0.,1.,0.));
#10177=DIRECTION('center_axis',(0.,-1.,0.));
#10178=DIRECTION('ref_axis',(1.,0.,0.));
#10179=DIRECTION('center_axis',(0.,1.,0.));
#10180=DIRECTION('ref_axis',(1.,0.,0.));
#10181=DIRECTION('center_axis',(0.,1.,0.));
#10182=DIRECTION('ref_axis',(1.,0.,0.));
#10183=DIRECTION('',(0.,1.,0.));
#10184=DIRECTION('center_axis',(0.,-1.,0.));
#10185=DIRECTION('ref_axis',(1.,0.,0.));
#10186=DIRECTION('center_axis',(0.,1.,0.));
#10187=DIRECTION('ref_axis',(1.,0.,0.));
#10188=DIRECTION('center_axis',(0.,1.,0.));
#10189=DIRECTION('ref_axis',(1.,0.,0.));
#10190=DIRECTION('',(0.,1.,0.));
#10191=DIRECTION('center_axis',(0.,-1.,0.));
#10192=DIRECTION('ref_axis',(1.,0.,0.));
#10193=DIRECTION('center_axis',(0.,1.,0.));
#10194=DIRECTION('ref_axis',(1.,0.,0.));
#10195=DIRECTION('center_axis',(0.,1.,0.));
#10196=DIRECTION('ref_axis',(1.,0.,0.));
#10197=DIRECTION('',(0.,1.,0.));
#10198=DIRECTION('center_axis',(0.,-1.,0.));
#10199=DIRECTION('ref_axis',(1.,0.,0.));
#10200=DIRECTION('center_axis',(0.,1.,0.));
#10201=DIRECTION('ref_axis',(1.,0.,0.));
#10202=DIRECTION('center_axis',(0.,1.,0.));
#10203=DIRECTION('ref_axis',(1.,0.,0.));
#10204=DIRECTION('',(0.,-1.,0.));
#10205=DIRECTION('center_axis',(0.,-1.,0.));
#10206=DIRECTION('ref_axis',(1.,0.,0.));
#10207=DIRECTION('center_axis',(0.,1.,0.));
#10208=DIRECTION('ref_axis',(1.,0.,0.));
#10209=DIRECTION('center_axis',(0.,-1.,0.));
#10210=DIRECTION('ref_axis',(1.,0.,0.));
#10211=DIRECTION('center_axis',(0.,1.,0.));
#10212=DIRECTION('ref_axis',(1.,0.,0.));
#10213=DIRECTION('',(0.,-1.,0.));
#10214=DIRECTION('center_axis',(0.,-1.,0.));
#10215=DIRECTION('ref_axis',(1.,0.,0.));
#10216=DIRECTION('center_axis',(0.,1.,0.));
#10217=DIRECTION('ref_axis',(1.,0.,0.));
#10218=DIRECTION('center_axis',(0.,1.,0.));
#10219=DIRECTION('ref_axis',(1.,0.,0.));
#10220=DIRECTION('',(0.,-1.,0.));
#10221=DIRECTION('center_axis',(0.,1.,0.));
#10222=DIRECTION('ref_axis',(1.,0.,0.));
#10223=DIRECTION('center_axis',(0.,1.,0.));
#10224=DIRECTION('ref_axis',(1.,0.,0.));
#10225=DIRECTION('center_axis',(0.,1.,0.));
#10226=DIRECTION('ref_axis',(1.,0.,0.));
#10227=DIRECTION('axis',(0.,0.,1.));
#10228=DIRECTION('refdir',(1.,0.,0.));
#10229=DIRECTION('center_axis',(0.,1.,0.));
#10230=DIRECTION('ref_axis',(1.,0.,0.));
#10231=DIRECTION('center_axis',(0.,1.,0.));
#10232=DIRECTION('ref_axis',(1.,0.,0.));
#10233=DIRECTION('',(0.,1.,0.));
#10234=DIRECTION('center_axis',(0.,-1.,0.));
#10235=DIRECTION('ref_axis',(1.,0.,0.));
#10236=DIRECTION('center_axis',(0.,1.,0.));
#10237=DIRECTION('ref_axis',(1.,0.,0.));
#10238=DIRECTION('center_axis',(0.,1.,0.));
#10239=DIRECTION('ref_axis',(1.,0.,0.));
#10240=DIRECTION('',(0.,1.,0.));
#10241=DIRECTION('center_axis',(0.,-1.,0.));
#10242=DIRECTION('ref_axis',(1.,0.,0.));
#10243=DIRECTION('center_axis',(0.,1.,0.));
#10244=DIRECTION('ref_axis',(1.,0.,0.));
#10245=DIRECTION('center_axis',(0.,1.,0.));
#10246=DIRECTION('ref_axis',(1.,0.,0.));
#10247=DIRECTION('',(0.,1.,0.));
#10248=DIRECTION('center_axis',(0.,-1.,0.));
#10249=DIRECTION('ref_axis',(1.,0.,0.));
#10250=DIRECTION('center_axis',(0.,1.,0.));
#10251=DIRECTION('ref_axis',(1.,0.,0.));
#10252=DIRECTION('center_axis',(0.,1.,0.));
#10253=DIRECTION('ref_axis',(1.,0.,0.));
#10254=DIRECTION('',(0.,1.,0.));
#10255=DIRECTION('center_axis',(0.,-1.,0.));
#10256=DIRECTION('ref_axis',(1.,0.,0.));
#10257=DIRECTION('center_axis',(0.,1.,0.));
#10258=DIRECTION('ref_axis',(1.,0.,0.));
#10259=DIRECTION('center_axis',(0.,1.,0.));
#10260=DIRECTION('ref_axis',(1.,0.,0.));
#10261=DIRECTION('',(0.,-1.,0.));
#10262=DIRECTION('center_axis',(0.,1.,0.));
#10263=DIRECTION('ref_axis',(1.,0.,0.));
#10264=DIRECTION('center_axis',(0.,1.,0.));
#10265=DIRECTION('ref_axis',(1.,0.,0.));
#10266=DIRECTION('center_axis',(0.,-1.,0.));
#10267=DIRECTION('ref_axis',(1.,0.,0.));
#10268=DIRECTION('center_axis',(0.,1.,0.));
#10269=DIRECTION('ref_axis',(1.,0.,0.));
#10270=DIRECTION('center_axis',(0.,-1.,0.));
#10271=DIRECTION('ref_axis',(1.,0.,0.));
#10272=DIRECTION('',(0.,-1.,0.));
#10273=DIRECTION('center_axis',(0.,1.,0.));
#10274=DIRECTION('ref_axis',(1.,0.,0.));
#10275=DIRECTION('center_axis',(0.,1.,0.));
#10276=DIRECTION('ref_axis',(1.,0.,0.));
#10277=DIRECTION('',(0.,-1.,0.));
#10278=DIRECTION('center_axis',(0.,1.,0.));
#10279=DIRECTION('ref_axis',(1.,0.,0.));
#10280=DIRECTION('center_axis',(0.,1.,0.));
#10281=DIRECTION('ref_axis',(1.,0.,0.));
#10282=DIRECTION('center_axis',(0.,1.,0.));
#10283=DIRECTION('ref_axis',(1.,0.,0.));
#10284=DIRECTION('axis',(0.,0.,1.));
#10285=DIRECTION('refdir',(1.,0.,0.));
#10286=DIRECTION('center_axis',(0.,1.,0.));
#10287=DIRECTION('ref_axis',(1.,0.,0.));
#10288=DIRECTION('center_axis',(0.,1.,0.));
#10289=DIRECTION('ref_axis',(1.,0.,0.));
#10290=DIRECTION('',(0.,1.,0.));
#10291=DIRECTION('center_axis',(0.,-1.,0.));
#10292=DIRECTION('ref_axis',(1.,0.,0.));
#10293=DIRECTION('center_axis',(0.,1.,0.));
#10294=DIRECTION('ref_axis',(1.,0.,0.));
#10295=DIRECTION('center_axis',(0.,1.,0.));
#10296=DIRECTION('ref_axis',(1.,0.,0.));
#10297=DIRECTION('',(0.,1.,0.));
#10298=DIRECTION('center_axis',(0.,-1.,0.));
#10299=DIRECTION('ref_axis',(1.,0.,0.));
#10300=DIRECTION('center_axis',(0.,1.,0.));
#10301=DIRECTION('ref_axis',(1.,0.,0.));
#10302=DIRECTION('center_axis',(0.,1.,0.));
#10303=DIRECTION('ref_axis',(1.,0.,0.));
#10304=DIRECTION('',(0.,1.,0.));
#10305=DIRECTION('center_axis',(0.,-1.,0.));
#10306=DIRECTION('ref_axis',(1.,0.,0.));
#10307=DIRECTION('center_axis',(0.,1.,0.));
#10308=DIRECTION('ref_axis',(1.,0.,0.));
#10309=DIRECTION('center_axis',(0.,1.,0.));
#10310=DIRECTION('ref_axis',(1.,0.,0.));
#10311=DIRECTION('',(0.,1.,0.));
#10312=DIRECTION('center_axis',(0.,-1.,0.));
#10313=DIRECTION('ref_axis',(1.,0.,0.));
#10314=DIRECTION('center_axis',(0.,1.,0.));
#10315=DIRECTION('ref_axis',(1.,0.,0.));
#10316=DIRECTION('center_axis',(0.,1.,0.));
#10317=DIRECTION('ref_axis',(1.,0.,0.));
#10318=DIRECTION('',(0.,1.,0.));
#10319=DIRECTION('center_axis',(0.,-1.,0.));
#10320=DIRECTION('ref_axis',(1.,0.,0.));
#10321=DIRECTION('center_axis',(0.,0.,1.));
#10322=DIRECTION('ref_axis',(1.,0.,0.));
#10323=DIRECTION('center_axis',(0.,0.,1.));
#10324=DIRECTION('ref_axis',(1.,0.,0.));
#10325=DIRECTION('',(0.,0.,1.));
#10326=DIRECTION('center_axis',(0.,0.,-1.));
#10327=DIRECTION('ref_axis',(1.,0.,0.));
#10328=DIRECTION('center_axis',(0.,0.,1.));
#10329=DIRECTION('ref_axis',(1.,0.,0.));
#10330=DIRECTION('center_axis',(0.,0.,1.));
#10331=DIRECTION('ref_axis',(1.,0.,0.));
#10332=DIRECTION('',(0.,0.,1.));
#10333=DIRECTION('center_axis',(0.,0.,-1.));
#10334=DIRECTION('ref_axis',(1.,0.,0.));
#10335=DIRECTION('center_axis',(0.,0.,1.));
#10336=DIRECTION('ref_axis',(1.,0.,0.));
#10337=DIRECTION('',(0.,1.,0.));
#10338=DIRECTION('',(-1.,0.,0.));
#10339=DIRECTION('',(0.,1.,0.));
#10340=DIRECTION('',(1.,0.,0.));
#10341=DIRECTION('center_axis',(0.,0.,1.));
#10342=DIRECTION('ref_axis',(1.,0.,0.));
#10343=DIRECTION('',(0.,-1.,0.));
#10344=DIRECTION('',(1.,0.,0.));
#10345=DIRECTION('',(0.,1.,0.));
#10346=DIRECTION('',(-1.,0.,0.));
#10347=DIRECTION('center_axis',(-1.,0.,0.));
#10348=DIRECTION('ref_axis',(0.,0.,1.));
#10349=DIRECTION('',(0.,0.,-1.));
#10350=DIRECTION('',(0.,0.,1.));
#10351=DIRECTION('',(0.,1.,0.));
#10352=DIRECTION('center_axis',(1.,0.,0.));
#10353=DIRECTION('ref_axis',(0.,0.,-1.));
#10354=DIRECTION('',(0.,0.,1.));
#10355=DIRECTION('',(0.,1.,0.));
#10356=DIRECTION('',(0.,0.,-1.));
#10357=DIRECTION('center_axis',(0.,-1.,0.));
#10358=DIRECTION('ref_axis',(1.,0.,0.));
#10359=DIRECTION('',(0.,0.,1.));
#10360=DIRECTION('',(1.,0.,0.));
#10361=DIRECTION('',(0.,0.,1.));
#10362=DIRECTION('',(1.,0.,0.));
#10363=DIRECTION('center_axis',(1.,0.,0.));
#10364=DIRECTION('ref_axis',(0.,1.,0.));
#10365=DIRECTION('',(0.,0.,1.));
#10366=DIRECTION('',(0.,1.,0.));
#10367=DIRECTION('center_axis',(0.,1.,0.));
#10368=DIRECTION('ref_axis',(-1.,0.,0.));
#10369=DIRECTION('',(0.,0.,1.));
#10370=DIRECTION('',(-1.,0.,0.));
#10371=DIRECTION('',(-1.,0.,0.));
#10372=DIRECTION('center_axis',(-1.,0.,0.));
#10373=DIRECTION('ref_axis',(0.,-1.,0.));
#10374=DIRECTION('',(0.,-1.,0.));
#10375=DIRECTION('center_axis',(0.,0.,1.));
#10376=DIRECTION('ref_axis',(1.,0.,0.));
#10377=DIRECTION('center_axis',(0.,0.,1.));
#10378=DIRECTION('ref_axis',(1.,0.,0.));
#10379=DIRECTION('axis',(0.,0.,1.));
#10380=DIRECTION('refdir',(1.,0.,0.));
#10381=DIRECTION('center_axis',(0.,1.,0.));
#10382=DIRECTION('ref_axis',(1.,0.,0.));
#10383=DIRECTION('center_axis',(0.,1.,0.));
#10384=DIRECTION('ref_axis',(1.,0.,0.));
#10385=DIRECTION('',(0.,1.,0.));
#10386=DIRECTION('center_axis',(0.,-1.,0.));
#10387=DIRECTION('ref_axis',(1.,0.,0.));
#10388=DIRECTION('center_axis',(0.,1.,0.));
#10389=DIRECTION('ref_axis',(1.,0.,0.));
#10390=DIRECTION('center_axis',(0.,1.,0.));
#10391=DIRECTION('ref_axis',(1.,0.,0.));
#10392=DIRECTION('',(0.,1.,0.));
#10393=DIRECTION('center_axis',(0.,-1.,0.));
#10394=DIRECTION('ref_axis',(1.,0.,0.));
#10395=DIRECTION('center_axis',(0.,1.,0.));
#10396=DIRECTION('ref_axis',(1.,0.,0.));
#10397=DIRECTION('center_axis',(0.,1.,0.));
#10398=DIRECTION('ref_axis',(1.,0.,0.));
#10399=DIRECTION('',(0.,1.,0.));
#10400=DIRECTION('center_axis',(0.,-1.,0.));
#10401=DIRECTION('ref_axis',(1.,0.,0.));
#10402=DIRECTION('center_axis',(0.,1.,0.));
#10403=DIRECTION('ref_axis',(1.,0.,0.));
#10404=DIRECTION('center_axis',(0.,1.,0.));
#10405=DIRECTION('ref_axis',(1.,0.,0.));
#10406=DIRECTION('',(0.,1.,0.));
#10407=DIRECTION('center_axis',(0.,-1.,0.));
#10408=DIRECTION('ref_axis',(1.,0.,0.));
#10409=DIRECTION('center_axis',(0.,1.,0.));
#10410=DIRECTION('ref_axis',(1.,0.,0.));
#10411=DIRECTION('center_axis',(0.,1.,0.));
#10412=DIRECTION('ref_axis',(1.,0.,0.));
#10413=DIRECTION('',(0.,-1.,0.));
#10414=DIRECTION('center_axis',(0.,-1.,0.));
#10415=DIRECTION('ref_axis',(1.,0.,0.));
#10416=DIRECTION('center_axis',(0.,1.,0.));
#10417=DIRECTION('ref_axis',(1.,0.,0.));
#10418=DIRECTION('center_axis',(0.,-1.,0.));
#10419=DIRECTION('ref_axis',(1.,0.,0.));
#10420=DIRECTION('center_axis',(0.,1.,0.));
#10421=DIRECTION('ref_axis',(1.,0.,0.));
#10422=DIRECTION('',(0.,-1.,0.));
#10423=DIRECTION('center_axis',(0.,-1.,0.));
#10424=DIRECTION('ref_axis',(1.,0.,0.));
#10425=DIRECTION('center_axis',(0.,1.,0.));
#10426=DIRECTION('ref_axis',(1.,0.,0.));
#10427=DIRECTION('center_axis',(0.,1.,0.));
#10428=DIRECTION('ref_axis',(1.,0.,0.));
#10429=DIRECTION('',(0.,-1.,0.));
#10430=DIRECTION('center_axis',(0.,1.,0.));
#10431=DIRECTION('ref_axis',(1.,0.,0.));
#10432=DIRECTION('center_axis',(0.,1.,0.));
#10433=DIRECTION('ref_axis',(1.,0.,0.));
#10434=DIRECTION('center_axis',(0.,1.,0.));
#10435=DIRECTION('ref_axis',(1.,0.,0.));
#10436=DIRECTION('axis',(0.,0.,1.));
#10437=DIRECTION('refdir',(1.,0.,0.));
#10438=DIRECTION('center_axis',(0.,1.,0.));
#10439=DIRECTION('ref_axis',(1.,0.,0.));
#10440=DIRECTION('center_axis',(0.,1.,0.));
#10441=DIRECTION('ref_axis',(1.,0.,0.));
#10442=DIRECTION('',(0.,1.,0.));
#10443=DIRECTION('center_axis',(0.,-1.,0.));
#10444=DIRECTION('ref_axis',(1.,0.,0.));
#10445=DIRECTION('center_axis',(0.,1.,0.));
#10446=DIRECTION('ref_axis',(1.,0.,0.));
#10447=DIRECTION('center_axis',(0.,1.,0.));
#10448=DIRECTION('ref_axis',(1.,0.,0.));
#10449=DIRECTION('',(0.,1.,0.));
#10450=DIRECTION('center_axis',(0.,-1.,0.));
#10451=DIRECTION('ref_axis',(1.,0.,0.));
#10452=DIRECTION('center_axis',(0.,1.,0.));
#10453=DIRECTION('ref_axis',(1.,0.,0.));
#10454=DIRECTION('center_axis',(0.,1.,0.));
#10455=DIRECTION('ref_axis',(1.,0.,0.));
#10456=DIRECTION('',(0.,1.,0.));
#10457=DIRECTION('center_axis',(0.,-1.,0.));
#10458=DIRECTION('ref_axis',(1.,0.,0.));
#10459=DIRECTION('center_axis',(0.,1.,0.));
#10460=DIRECTION('ref_axis',(1.,0.,0.));
#10461=DIRECTION('center_axis',(0.,1.,0.));
#10462=DIRECTION('ref_axis',(1.,0.,0.));
#10463=DIRECTION('',(0.,1.,0.));
#10464=DIRECTION('center_axis',(0.,-1.,0.));
#10465=DIRECTION('ref_axis',(1.,0.,0.));
#10466=DIRECTION('center_axis',(0.,1.,0.));
#10467=DIRECTION('ref_axis',(1.,0.,0.));
#10468=DIRECTION('center_axis',(0.,1.,0.));
#10469=DIRECTION('ref_axis',(1.,0.,0.));
#10470=DIRECTION('',(0.,-1.,0.));
#10471=DIRECTION('center_axis',(0.,1.,0.));
#10472=DIRECTION('ref_axis',(1.,0.,0.));
#10473=DIRECTION('center_axis',(0.,1.,0.));
#10474=DIRECTION('ref_axis',(1.,0.,0.));
#10475=DIRECTION('center_axis',(0.,-1.,0.));
#10476=DIRECTION('ref_axis',(1.,0.,0.));
#10477=DIRECTION('center_axis',(0.,1.,0.));
#10478=DIRECTION('ref_axis',(1.,0.,0.));
#10479=DIRECTION('center_axis',(0.,-1.,0.));
#10480=DIRECTION('ref_axis',(1.,0.,0.));
#10481=DIRECTION('',(0.,-1.,0.));
#10482=DIRECTION('center_axis',(0.,1.,0.));
#10483=DIRECTION('ref_axis',(1.,0.,0.));
#10484=DIRECTION('center_axis',(0.,1.,0.));
#10485=DIRECTION('ref_axis',(1.,0.,0.));
#10486=DIRECTION('',(0.,-1.,0.));
#10487=DIRECTION('center_axis',(0.,1.,0.));
#10488=DIRECTION('ref_axis',(1.,0.,0.));
#10489=DIRECTION('center_axis',(0.,1.,0.));
#10490=DIRECTION('ref_axis',(1.,0.,0.));
#10491=DIRECTION('center_axis',(0.,1.,0.));
#10492=DIRECTION('ref_axis',(1.,0.,0.));
#10493=DIRECTION('axis',(0.,0.,1.));
#10494=DIRECTION('refdir',(1.,0.,0.));
#10495=DIRECTION('center_axis',(1.,0.,0.));
#10496=DIRECTION('ref_axis',(0.,0.,-1.));
#10497=DIRECTION('center_axis',(1.,0.,0.));
#10498=DIRECTION('ref_axis',(0.,0.,-1.));
#10499=DIRECTION('',(1.,0.,0.));
#10500=DIRECTION('center_axis',(-1.,0.,0.));
#10501=DIRECTION('ref_axis',(0.,0.,-1.));
#10502=DIRECTION('center_axis',(1.,0.,0.));
#10503=DIRECTION('ref_axis',(0.,0.,-1.));
#10504=DIRECTION('center_axis',(1.,0.,0.));
#10505=DIRECTION('ref_axis',(0.,0.,-1.));
#10506=DIRECTION('',(1.,0.,0.));
#10507=DIRECTION('center_axis',(-1.,0.,0.));
#10508=DIRECTION('ref_axis',(0.,0.,-1.));
#10509=DIRECTION('center_axis',(1.,0.,0.));
#10510=DIRECTION('ref_axis',(0.,0.,-1.));
#10511=DIRECTION('center_axis',(1.,0.,0.));
#10512=DIRECTION('ref_axis',(0.,0.,-1.));
#10513=DIRECTION('',(1.,0.,0.));
#10514=DIRECTION('center_axis',(-1.,0.,0.));
#10515=DIRECTION('ref_axis',(0.,0.,-1.));
#10516=DIRECTION('center_axis',(1.,0.,0.));
#10517=DIRECTION('ref_axis',(0.,0.,-1.));
#10518=DIRECTION('center_axis',(1.,0.,0.));
#10519=DIRECTION('ref_axis',(0.,0.,-1.));
#10520=DIRECTION('',(1.,0.,0.));
#10521=DIRECTION('center_axis',(-1.,0.,0.));
#10522=DIRECTION('ref_axis',(0.,0.,-1.));
#10523=DIRECTION('center_axis',(1.,0.,0.));
#10524=DIRECTION('ref_axis',(0.,0.,-1.));
#10525=DIRECTION('center_axis',(1.,0.,0.));
#10526=DIRECTION('ref_axis',(0.,0.,-1.));
#10527=DIRECTION('',(1.,0.,0.));
#10528=DIRECTION('center_axis',(-1.,0.,0.));
#10529=DIRECTION('ref_axis',(0.,0.,-1.));
#10530=DIRECTION('center_axis',(0.,0.,1.));
#10531=DIRECTION('ref_axis',(1.,0.,0.));
#10532=DIRECTION('center_axis',(0.,0.,1.));
#10533=DIRECTION('ref_axis',(1.,0.,0.));
#10534=DIRECTION('',(0.,0.,1.));
#10535=DIRECTION('center_axis',(0.,0.,-1.));
#10536=DIRECTION('ref_axis',(1.,0.,0.));
#10537=DIRECTION('center_axis',(0.,0.,1.));
#10538=DIRECTION('ref_axis',(1.,0.,0.));
#10539=DIRECTION('center_axis',(0.,0.,1.));
#10540=DIRECTION('ref_axis',(1.,0.,0.));
#10541=DIRECTION('',(0.,0.,1.));
#10542=DIRECTION('center_axis',(0.,0.,-1.));
#10543=DIRECTION('ref_axis',(1.,0.,0.));
#10544=DIRECTION('center_axis',(0.,0.,1.));
#10545=DIRECTION('ref_axis',(1.,0.,0.));
#10546=DIRECTION('',(0.,1.,0.));
#10547=DIRECTION('',(-1.,0.,0.));
#10548=DIRECTION('',(0.,1.,0.));
#10549=DIRECTION('',(1.,0.,0.));
#10550=DIRECTION('center_axis',(0.,0.,1.));
#10551=DIRECTION('ref_axis',(1.,0.,0.));
#10552=DIRECTION('',(0.,-1.,0.));
#10553=DIRECTION('',(1.,0.,0.));
#10554=DIRECTION('',(0.,1.,0.));
#10555=DIRECTION('',(-1.,0.,0.));
#10556=DIRECTION('center_axis',(-1.,0.,0.));
#10557=DIRECTION('ref_axis',(0.,0.,1.));
#10558=DIRECTION('',(0.,0.,-1.));
#10559=DIRECTION('',(0.,0.,1.));
#10560=DIRECTION('',(0.,1.,0.));
#10561=DIRECTION('center_axis',(1.,0.,0.));
#10562=DIRECTION('ref_axis',(0.,0.,-1.));
#10563=DIRECTION('',(0.,0.,1.));
#10564=DIRECTION('',(0.,1.,0.));
#10565=DIRECTION('',(0.,0.,-1.));
#10566=DIRECTION('center_axis',(0.,-1.,0.));
#10567=DIRECTION('ref_axis',(1.,0.,0.));
#10568=DIRECTION('',(0.,0.,1.));
#10569=DIRECTION('',(1.,0.,0.));
#10570=DIRECTION('',(0.,0.,1.));
#10571=DIRECTION('',(1.,0.,0.));
#10572=DIRECTION('center_axis',(1.,0.,0.));
#10573=DIRECTION('ref_axis',(0.,1.,0.));
#10574=DIRECTION('',(0.,0.,1.));
#10575=DIRECTION('',(0.,1.,0.));
#10576=DIRECTION('center_axis',(0.,1.,0.));
#10577=DIRECTION('ref_axis',(-1.,0.,0.));
#10578=DIRECTION('',(0.,0.,1.));
#10579=DIRECTION('',(-1.,0.,0.));
#10580=DIRECTION('',(-1.,0.,0.));
#10581=DIRECTION('center_axis',(-1.,0.,0.));
#10582=DIRECTION('ref_axis',(0.,-1.,0.));
#10583=DIRECTION('',(0.,-1.,0.));
#10584=DIRECTION('center_axis',(0.,0.,1.));
#10585=DIRECTION('ref_axis',(1.,0.,0.));
#10586=DIRECTION('center_axis',(0.,0.,1.));
#10587=DIRECTION('ref_axis',(1.,0.,0.));
#10588=DIRECTION('axis',(0.,0.,1.));
#10589=DIRECTION('refdir',(1.,0.,0.));
#10590=DIRECTION('center_axis',(1.,0.,0.));
#10591=DIRECTION('ref_axis',(0.,0.,-1.));
#10592=DIRECTION('center_axis',(1.,0.,0.));
#10593=DIRECTION('ref_axis',(0.,0.,-1.));
#10594=DIRECTION('',(1.,0.,0.));
#10595=DIRECTION('center_axis',(-1.,0.,0.));
#10596=DIRECTION('ref_axis',(0.,0.,-1.));
#10597=DIRECTION('center_axis',(1.,0.,0.));
#10598=DIRECTION('ref_axis',(0.,0.,-1.));
#10599=DIRECTION('center_axis',(1.,0.,0.));
#10600=DIRECTION('ref_axis',(0.,0.,-1.));
#10601=DIRECTION('',(1.,0.,0.));
#10602=DIRECTION('center_axis',(-1.,0.,0.));
#10603=DIRECTION('ref_axis',(0.,0.,-1.));
#10604=DIRECTION('center_axis',(1.,0.,0.));
#10605=DIRECTION('ref_axis',(0.,0.,-1.));
#10606=DIRECTION('center_axis',(1.,0.,0.));
#10607=DIRECTION('ref_axis',(0.,0.,-1.));
#10608=DIRECTION('',(1.,0.,0.));
#10609=DIRECTION('center_axis',(-1.,0.,0.));
#10610=DIRECTION('ref_axis',(0.,0.,-1.));
#10611=DIRECTION('center_axis',(1.,0.,0.));
#10612=DIRECTION('ref_axis',(0.,0.,-1.));
#10613=DIRECTION('center_axis',(1.,0.,0.));
#10614=DIRECTION('ref_axis',(0.,0.,-1.));
#10615=DIRECTION('',(1.,0.,0.));
#10616=DIRECTION('center_axis',(-1.,0.,0.));
#10617=DIRECTION('ref_axis',(0.,0.,-1.));
#10618=DIRECTION('center_axis',(1.,0.,0.));
#10619=DIRECTION('ref_axis',(0.,0.,-1.));
#10620=DIRECTION('center_axis',(1.,0.,0.));
#10621=DIRECTION('ref_axis',(0.,0.,-1.));
#10622=DIRECTION('',(-1.,0.,0.));
#10623=DIRECTION('center_axis',(-1.,0.,0.));
#10624=DIRECTION('ref_axis',(0.,0.,-1.));
#10625=DIRECTION('center_axis',(1.,0.,0.));
#10626=DIRECTION('ref_axis',(0.,0.,-1.));
#10627=DIRECTION('center_axis',(-1.,0.,0.));
#10628=DIRECTION('ref_axis',(0.,0.,-1.));
#10629=DIRECTION('center_axis',(1.,0.,0.));
#10630=DIRECTION('ref_axis',(0.,0.,-1.));
#10631=DIRECTION('',(-1.,0.,0.));
#10632=DIRECTION('center_axis',(-1.,0.,0.));
#10633=DIRECTION('ref_axis',(0.,0.,-1.));
#10634=DIRECTION('center_axis',(1.,0.,0.));
#10635=DIRECTION('ref_axis',(0.,0.,-1.));
#10636=DIRECTION('center_axis',(1.,0.,0.));
#10637=DIRECTION('ref_axis',(0.,0.,-1.));
#10638=DIRECTION('',(-1.,0.,0.));
#10639=DIRECTION('center_axis',(1.,0.,0.));
#10640=DIRECTION('ref_axis',(0.,0.,-1.));
#10641=DIRECTION('center_axis',(1.,0.,0.));
#10642=DIRECTION('ref_axis',(0.,0.,-1.));
#10643=DIRECTION('center_axis',(1.,0.,0.));
#10644=DIRECTION('ref_axis',(0.,0.,-1.));
#10645=DIRECTION('axis',(0.,0.,1.));
#10646=DIRECTION('refdir',(1.,0.,0.));
#10647=DIRECTION('center_axis',(1.,0.,0.));
#10648=DIRECTION('ref_axis',(0.,0.,-1.));
#10649=DIRECTION('center_axis',(1.,0.,0.));
#10650=DIRECTION('ref_axis',(0.,0.,-1.));
#10651=DIRECTION('',(1.,0.,0.));
#10652=DIRECTION('center_axis',(-1.,0.,0.));
#10653=DIRECTION('ref_axis',(0.,0.,-1.));
#10654=DIRECTION('center_axis',(1.,0.,0.));
#10655=DIRECTION('ref_axis',(0.,0.,-1.));
#10656=DIRECTION('center_axis',(1.,0.,0.));
#10657=DIRECTION('ref_axis',(0.,0.,-1.));
#10658=DIRECTION('',(1.,0.,0.));
#10659=DIRECTION('center_axis',(-1.,0.,0.));
#10660=DIRECTION('ref_axis',(0.,0.,-1.));
#10661=DIRECTION('center_axis',(1.,0.,0.));
#10662=DIRECTION('ref_axis',(0.,0.,-1.));
#10663=DIRECTION('center_axis',(1.,0.,0.));
#10664=DIRECTION('ref_axis',(0.,0.,-1.));
#10665=DIRECTION('',(1.,0.,0.));
#10666=DIRECTION('center_axis',(-1.,0.,0.));
#10667=DIRECTION('ref_axis',(0.,0.,-1.));
#10668=DIRECTION('center_axis',(1.,0.,0.));
#10669=DIRECTION('ref_axis',(0.,0.,-1.));
#10670=DIRECTION('center_axis',(1.,0.,0.));
#10671=DIRECTION('ref_axis',(0.,0.,-1.));
#10672=DIRECTION('',(1.,0.,0.));
#10673=DIRECTION('center_axis',(-1.,0.,0.));
#10674=DIRECTION('ref_axis',(0.,0.,-1.));
#10675=DIRECTION('center_axis',(1.,0.,0.));
#10676=DIRECTION('ref_axis',(0.,0.,-1.));
#10677=DIRECTION('center_axis',(1.,0.,0.));
#10678=DIRECTION('ref_axis',(0.,0.,-1.));
#10679=DIRECTION('',(-1.,0.,0.));
#10680=DIRECTION('center_axis',(1.,0.,0.));
#10681=DIRECTION('ref_axis',(0.,0.,-1.));
#10682=DIRECTION('center_axis',(1.,0.,0.));
#10683=DIRECTION('ref_axis',(0.,0.,-1.));
#10684=DIRECTION('center_axis',(-1.,0.,0.));
#10685=DIRECTION('ref_axis',(0.,0.,-1.));
#10686=DIRECTION('center_axis',(1.,0.,0.));
#10687=DIRECTION('ref_axis',(0.,0.,-1.));
#10688=DIRECTION('center_axis',(-1.,0.,0.));
#10689=DIRECTION('ref_axis',(0.,0.,-1.));
#10690=DIRECTION('',(-1.,0.,0.));
#10691=DIRECTION('center_axis',(1.,0.,0.));
#10692=DIRECTION('ref_axis',(0.,0.,-1.));
#10693=DIRECTION('center_axis',(1.,0.,0.));
#10694=DIRECTION('ref_axis',(0.,0.,-1.));
#10695=DIRECTION('',(-1.,0.,0.));
#10696=DIRECTION('center_axis',(1.,0.,0.));
#10697=DIRECTION('ref_axis',(0.,0.,-1.));
#10698=DIRECTION('center_axis',(1.,0.,0.));
#10699=DIRECTION('ref_axis',(0.,0.,-1.));
#10700=DIRECTION('center_axis',(1.,0.,0.));
#10701=DIRECTION('ref_axis',(0.,0.,-1.));
#10702=DIRECTION('axis',(0.,0.,1.));
#10703=DIRECTION('refdir',(1.,0.,0.));
#10704=DIRECTION('center_axis',(1.,0.,0.));
#10705=DIRECTION('ref_axis',(0.,0.,-1.));
#10706=DIRECTION('center_axis',(1.,0.,0.));
#10707=DIRECTION('ref_axis',(0.,0.,-1.));
#10708=DIRECTION('',(1.,0.,0.));
#10709=DIRECTION('center_axis',(-1.,0.,0.));
#10710=DIRECTION('ref_axis',(0.,0.,-1.));
#10711=DIRECTION('center_axis',(1.,0.,0.));
#10712=DIRECTION('ref_axis',(0.,0.,-1.));
#10713=DIRECTION('center_axis',(1.,0.,0.));
#10714=DIRECTION('ref_axis',(0.,0.,-1.));
#10715=DIRECTION('',(1.,0.,0.));
#10716=DIRECTION('center_axis',(-1.,0.,0.));
#10717=DIRECTION('ref_axis',(0.,0.,-1.));
#10718=DIRECTION('center_axis',(1.,0.,0.));
#10719=DIRECTION('ref_axis',(0.,0.,-1.));
#10720=DIRECTION('center_axis',(1.,0.,0.));
#10721=DIRECTION('ref_axis',(0.,0.,-1.));
#10722=DIRECTION('',(1.,0.,0.));
#10723=DIRECTION('center_axis',(-1.,0.,0.));
#10724=DIRECTION('ref_axis',(0.,0.,-1.));
#10725=DIRECTION('center_axis',(1.,0.,0.));
#10726=DIRECTION('ref_axis',(0.,0.,-1.));
#10727=DIRECTION('center_axis',(1.,0.,0.));
#10728=DIRECTION('ref_axis',(0.,0.,-1.));
#10729=DIRECTION('',(1.,0.,0.));
#10730=DIRECTION('center_axis',(-1.,0.,0.));
#10731=DIRECTION('ref_axis',(0.,0.,-1.));
#10732=DIRECTION('center_axis',(1.,0.,0.));
#10733=DIRECTION('ref_axis',(0.,0.,-1.));
#10734=DIRECTION('center_axis',(1.,0.,0.));
#10735=DIRECTION('ref_axis',(0.,0.,-1.));
#10736=DIRECTION('',(1.,0.,0.));
#10737=DIRECTION('center_axis',(-1.,0.,0.));
#10738=DIRECTION('ref_axis',(0.,0.,-1.));
#10739=DIRECTION('center_axis',(0.,0.,1.));
#10740=DIRECTION('ref_axis',(1.,0.,0.));
#10741=DIRECTION('center_axis',(0.,0.,1.));
#10742=DIRECTION('ref_axis',(1.,0.,0.));
#10743=DIRECTION('',(0.,0.,1.));
#10744=DIRECTION('center_axis',(0.,0.,-1.));
#10745=DIRECTION('ref_axis',(1.,0.,0.));
#10746=DIRECTION('center_axis',(0.,0.,1.));
#10747=DIRECTION('ref_axis',(1.,0.,0.));
#10748=DIRECTION('center_axis',(0.,0.,1.));
#10749=DIRECTION('ref_axis',(1.,0.,0.));
#10750=DIRECTION('',(0.,0.,1.));
#10751=DIRECTION('center_axis',(0.,0.,-1.));
#10752=DIRECTION('ref_axis',(1.,0.,0.));
#10753=DIRECTION('center_axis',(0.,0.,1.));
#10754=DIRECTION('ref_axis',(1.,0.,0.));
#10755=DIRECTION('',(0.,1.,0.));
#10756=DIRECTION('',(-1.,0.,0.));
#10757=DIRECTION('',(0.,1.,0.));
#10758=DIRECTION('',(1.,0.,0.));
#10759=DIRECTION('center_axis',(0.,0.,1.));
#10760=DIRECTION('ref_axis',(1.,0.,0.));
#10761=DIRECTION('',(0.,-1.,0.));
#10762=DIRECTION('',(1.,0.,0.));
#10763=DIRECTION('',(0.,1.,0.));
#10764=DIRECTION('',(-1.,0.,0.));
#10765=DIRECTION('center_axis',(-1.,0.,0.));
#10766=DIRECTION('ref_axis',(0.,0.,1.));
#10767=DIRECTION('',(0.,0.,-1.));
#10768=DIRECTION('',(0.,0.,1.));
#10769=DIRECTION('',(0.,1.,0.));
#10770=DIRECTION('center_axis',(1.,0.,0.));
#10771=DIRECTION('ref_axis',(0.,0.,-1.));
#10772=DIRECTION('',(0.,0.,1.));
#10773=DIRECTION('',(0.,1.,0.));
#10774=DIRECTION('',(0.,0.,-1.));
#10775=DIRECTION('center_axis',(0.,-1.,0.));
#10776=DIRECTION('ref_axis',(1.,0.,0.));
#10777=DIRECTION('',(0.,0.,1.));
#10778=DIRECTION('',(1.,0.,0.));
#10779=DIRECTION('',(0.,0.,1.));
#10780=DIRECTION('',(1.,0.,0.));
#10781=DIRECTION('center_axis',(1.,0.,0.));
#10782=DIRECTION('ref_axis',(0.,1.,0.));
#10783=DIRECTION('',(0.,0.,1.));
#10784=DIRECTION('',(0.,1.,0.));
#10785=DIRECTION('center_axis',(0.,1.,0.));
#10786=DIRECTION('ref_axis',(-1.,0.,0.));
#10787=DIRECTION('',(0.,0.,1.));
#10788=DIRECTION('',(-1.,0.,0.));
#10789=DIRECTION('',(-1.,0.,0.));
#10790=DIRECTION('center_axis',(-1.,0.,0.));
#10791=DIRECTION('ref_axis',(0.,-1.,0.));
#10792=DIRECTION('',(0.,-1.,0.));
#10793=DIRECTION('center_axis',(0.,0.,1.));
#10794=DIRECTION('ref_axis',(1.,0.,0.));
#10795=DIRECTION('center_axis',(0.,0.,1.));
#10796=DIRECTION('ref_axis',(1.,0.,0.));
#10797=DIRECTION('axis',(0.,0.,1.));
#10798=DIRECTION('refdir',(1.,0.,0.));
#10799=DIRECTION('center_axis',(1.,0.,0.));
#10800=DIRECTION('ref_axis',(0.,0.,-1.));
#10801=DIRECTION('center_axis',(1.,0.,0.));
#10802=DIRECTION('ref_axis',(0.,0.,-1.));
#10803=DIRECTION('',(1.,0.,0.));
#10804=DIRECTION('center_axis',(-1.,0.,0.));
#10805=DIRECTION('ref_axis',(0.,0.,-1.));
#10806=DIRECTION('center_axis',(1.,0.,0.));
#10807=DIRECTION('ref_axis',(0.,0.,-1.));
#10808=DIRECTION('center_axis',(1.,0.,0.));
#10809=DIRECTION('ref_axis',(0.,0.,-1.));
#10810=DIRECTION('',(1.,0.,0.));
#10811=DIRECTION('center_axis',(-1.,0.,0.));
#10812=DIRECTION('ref_axis',(0.,0.,-1.));
#10813=DIRECTION('center_axis',(1.,0.,0.));
#10814=DIRECTION('ref_axis',(0.,0.,-1.));
#10815=DIRECTION('center_axis',(1.,0.,0.));
#10816=DIRECTION('ref_axis',(0.,0.,-1.));
#10817=DIRECTION('',(1.,0.,0.));
#10818=DIRECTION('center_axis',(-1.,0.,0.));
#10819=DIRECTION('ref_axis',(0.,0.,-1.));
#10820=DIRECTION('center_axis',(1.,0.,0.));
#10821=DIRECTION('ref_axis',(0.,0.,-1.));
#10822=DIRECTION('center_axis',(1.,0.,0.));
#10823=DIRECTION('ref_axis',(0.,0.,-1.));
#10824=DIRECTION('',(1.,0.,0.));
#10825=DIRECTION('center_axis',(-1.,0.,0.));
#10826=DIRECTION('ref_axis',(0.,0.,-1.));
#10827=DIRECTION('center_axis',(1.,0.,0.));
#10828=DIRECTION('ref_axis',(0.,0.,-1.));
#10829=DIRECTION('center_axis',(1.,0.,0.));
#10830=DIRECTION('ref_axis',(0.,0.,-1.));
#10831=DIRECTION('',(-1.,0.,0.));
#10832=DIRECTION('center_axis',(-1.,0.,0.));
#10833=DIRECTION('ref_axis',(0.,0.,-1.));
#10834=DIRECTION('center_axis',(1.,0.,0.));
#10835=DIRECTION('ref_axis',(0.,0.,-1.));
#10836=DIRECTION('center_axis',(-1.,0.,0.));
#10837=DIRECTION('ref_axis',(0.,0.,-1.));
#10838=DIRECTION('center_axis',(1.,0.,0.));
#10839=DIRECTION('ref_axis',(0.,0.,-1.));
#10840=DIRECTION('',(-1.,0.,0.));
#10841=DIRECTION('center_axis',(-1.,0.,0.));
#10842=DIRECTION('ref_axis',(0.,0.,-1.));
#10843=DIRECTION('center_axis',(1.,0.,0.));
#10844=DIRECTION('ref_axis',(0.,0.,-1.));
#10845=DIRECTION('center_axis',(1.,0.,0.));
#10846=DIRECTION('ref_axis',(0.,0.,-1.));
#10847=DIRECTION('',(-1.,0.,0.));
#10848=DIRECTION('center_axis',(1.,0.,0.));
#10849=DIRECTION('ref_axis',(0.,0.,-1.));
#10850=DIRECTION('center_axis',(1.,0.,0.));
#10851=DIRECTION('ref_axis',(0.,0.,-1.));
#10852=DIRECTION('center_axis',(1.,0.,0.));
#10853=DIRECTION('ref_axis',(0.,0.,-1.));
#10854=DIRECTION('axis',(0.,0.,1.));
#10855=DIRECTION('refdir',(1.,0.,0.));
#10856=DIRECTION('center_axis',(1.,0.,0.));
#10857=DIRECTION('ref_axis',(0.,0.,-1.));
#10858=DIRECTION('center_axis',(1.,0.,0.));
#10859=DIRECTION('ref_axis',(0.,0.,-1.));
#10860=DIRECTION('',(1.,0.,0.));
#10861=DIRECTION('center_axis',(-1.,0.,0.));
#10862=DIRECTION('ref_axis',(0.,0.,-1.));
#10863=DIRECTION('center_axis',(1.,0.,0.));
#10864=DIRECTION('ref_axis',(0.,0.,-1.));
#10865=DIRECTION('center_axis',(1.,0.,0.));
#10866=DIRECTION('ref_axis',(0.,0.,-1.));
#10867=DIRECTION('',(1.,0.,0.));
#10868=DIRECTION('center_axis',(-1.,0.,0.));
#10869=DIRECTION('ref_axis',(0.,0.,-1.));
#10870=DIRECTION('center_axis',(1.,0.,0.));
#10871=DIRECTION('ref_axis',(0.,0.,-1.));
#10872=DIRECTION('center_axis',(1.,0.,0.));
#10873=DIRECTION('ref_axis',(0.,0.,-1.));
#10874=DIRECTION('',(1.,0.,0.));
#10875=DIRECTION('center_axis',(-1.,0.,0.));
#10876=DIRECTION('ref_axis',(0.,0.,-1.));
#10877=DIRECTION('center_axis',(1.,0.,0.));
#10878=DIRECTION('ref_axis',(0.,0.,-1.));
#10879=DIRECTION('center_axis',(1.,0.,0.));
#10880=DIRECTION('ref_axis',(0.,0.,-1.));
#10881=DIRECTION('',(1.,0.,0.));
#10882=DIRECTION('center_axis',(-1.,0.,0.));
#10883=DIRECTION('ref_axis',(0.,0.,-1.));
#10884=DIRECTION('center_axis',(1.,0.,0.));
#10885=DIRECTION('ref_axis',(0.,0.,-1.));
#10886=DIRECTION('center_axis',(1.,0.,0.));
#10887=DIRECTION('ref_axis',(0.,0.,-1.));
#10888=DIRECTION('',(-1.,0.,0.));
#10889=DIRECTION('center_axis',(1.,0.,0.));
#10890=DIRECTION('ref_axis',(0.,0.,-1.));
#10891=DIRECTION('center_axis',(1.,0.,0.));
#10892=DIRECTION('ref_axis',(0.,0.,-1.));
#10893=DIRECTION('center_axis',(-1.,0.,0.));
#10894=DIRECTION('ref_axis',(0.,0.,-1.));
#10895=DIRECTION('center_axis',(1.,0.,0.));
#10896=DIRECTION('ref_axis',(0.,0.,-1.));
#10897=DIRECTION('center_axis',(-1.,0.,0.));
#10898=DIRECTION('ref_axis',(0.,0.,-1.));
#10899=DIRECTION('',(-1.,0.,0.));
#10900=DIRECTION('center_axis',(1.,0.,0.));
#10901=DIRECTION('ref_axis',(0.,0.,-1.));
#10902=DIRECTION('center_axis',(1.,0.,0.));
#10903=DIRECTION('ref_axis',(0.,0.,-1.));
#10904=DIRECTION('',(-1.,0.,0.));
#10905=DIRECTION('center_axis',(1.,0.,0.));
#10906=DIRECTION('ref_axis',(0.,0.,-1.));
#10907=DIRECTION('center_axis',(1.,0.,0.));
#10908=DIRECTION('ref_axis',(0.,0.,-1.));
#10909=DIRECTION('center_axis',(1.,0.,0.));
#10910=DIRECTION('ref_axis',(0.,0.,-1.));
#10911=DIRECTION('axis',(0.,0.,1.));
#10912=DIRECTION('refdir',(1.,0.,0.));
#10913=DIRECTION('center_axis',(0.,1.,0.));
#10914=DIRECTION('ref_axis',(1.,0.,0.));
#10915=DIRECTION('center_axis',(0.,1.,0.));
#10916=DIRECTION('ref_axis',(1.,0.,0.));
#10917=DIRECTION('',(0.,1.,0.));
#10918=DIRECTION('center_axis',(0.,-1.,0.));
#10919=DIRECTION('ref_axis',(1.,0.,0.));
#10920=DIRECTION('center_axis',(0.,1.,0.));
#10921=DIRECTION('ref_axis',(1.,0.,0.));
#10922=DIRECTION('center_axis',(0.,1.,0.));
#10923=DIRECTION('ref_axis',(1.,0.,0.));
#10924=DIRECTION('',(0.,1.,0.));
#10925=DIRECTION('center_axis',(0.,-1.,0.));
#10926=DIRECTION('ref_axis',(1.,0.,0.));
#10927=DIRECTION('center_axis',(0.,0.,1.));
#10928=DIRECTION('ref_axis',(1.,0.,0.));
#10929=DIRECTION('center_axis',(0.,0.,1.));
#10930=DIRECTION('ref_axis',(1.,0.,0.));
#10931=DIRECTION('',(0.,0.,1.));
#10932=DIRECTION('center_axis',(0.,0.,-1.));
#10933=DIRECTION('ref_axis',(1.,0.,0.));
#10934=DIRECTION('center_axis',(0.,0.,1.));
#10935=DIRECTION('ref_axis',(1.,0.,0.));
#10936=DIRECTION('center_axis',(0.,0.,1.));
#10937=DIRECTION('ref_axis',(1.,0.,0.));
#10938=DIRECTION('center_axis',(0.,0.,1.));
#10939=DIRECTION('ref_axis',(1.,0.,0.));
#10940=DIRECTION('center_axis',(0.,0.,1.));
#10941=DIRECTION('ref_axis',(1.,0.,0.));
#10942=DIRECTION('',(0.,0.,1.));
#10943=DIRECTION('center_axis',(0.,0.,1.));
#10944=DIRECTION('ref_axis',(1.,0.,0.));
#10945=DIRECTION('center_axis',(0.,0.,1.));
#10946=DIRECTION('ref_axis',(1.,0.,0.));
#10947=DIRECTION('',(0.,0.,1.));
#10948=DIRECTION('center_axis',(0.,0.,-1.));
#10949=DIRECTION('ref_axis',(1.,0.,0.));
#10950=DIRECTION('center_axis',(0.,0.,1.));
#10951=DIRECTION('ref_axis',(1.,0.,0.));
#10952=DIRECTION('center_axis',(0.,0.,1.));
#10953=DIRECTION('ref_axis',(1.,0.,0.));
#10954=DIRECTION('center_axis',(0.,0.,1.));
#10955=DIRECTION('ref_axis',(1.,0.,0.));
#10956=DIRECTION('center_axis',(0.,0.,1.));
#10957=DIRECTION('ref_axis',(1.,0.,0.));
#10958=DIRECTION('',(0.,0.,1.));
#10959=DIRECTION('center_axis',(0.,1.,0.));
#10960=DIRECTION('ref_axis',(-1.,0.,0.));
#10961=DIRECTION('',(-1.,0.,0.));
#10962=DIRECTION('',(0.,0.,1.));
#10963=DIRECTION('',(-1.,0.,0.));
#10964=DIRECTION('',(0.,0.,1.));
#10965=DIRECTION('center_axis',(1.,0.,0.));
#10966=DIRECTION('ref_axis',(0.,1.,0.));
#10967=DIRECTION('',(0.,1.,0.));
#10968=DIRECTION('',(0.,1.,0.));
#10969=DIRECTION('',(0.,0.,1.));
#10970=DIRECTION('center_axis',(0.,-1.,0.));
#10971=DIRECTION('ref_axis',(1.,0.,0.));
#10972=DIRECTION('',(1.,0.,0.));
#10973=DIRECTION('',(1.,0.,0.));
#10974=DIRECTION('',(0.,0.,1.));
#10975=DIRECTION('center_axis',(-1.,0.,0.));
#10976=DIRECTION('ref_axis',(0.,-1.,0.));
#10977=DIRECTION('',(0.,-1.,0.));
#10978=DIRECTION('',(0.,-1.,0.));
#10979=DIRECTION('center_axis',(0.,0.,1.));
#10980=DIRECTION('ref_axis',(1.,0.,0.));
#10981=DIRECTION('center_axis',(0.,0.,1.));
#10982=DIRECTION('ref_axis',(1.,0.,0.));
#10983=DIRECTION('axis',(0.,0.,1.));
#10984=DIRECTION('refdir',(1.,0.,0.));
#10985=DIRECTION('center_axis',(0.,1.,0.));
#10986=DIRECTION('ref_axis',(1.,0.,0.));
#10987=DIRECTION('center_axis',(0.,1.,0.));
#10988=DIRECTION('ref_axis',(1.,0.,0.));
#10989=DIRECTION('',(0.,-1.,0.));
#10990=DIRECTION('center_axis',(0.,1.,0.));
#10991=DIRECTION('ref_axis',(1.,0.,0.));
#10992=DIRECTION('center_axis',(0.,1.,0.));
#10993=DIRECTION('ref_axis',(1.,0.,0.));
#10994=DIRECTION('center_axis',(0.,1.,0.));
#10995=DIRECTION('ref_axis',(1.,0.,0.));
#10996=DIRECTION('axis',(0.,0.,1.));
#10997=DIRECTION('refdir',(1.,0.,0.));
#10998=DIRECTION('center_axis',(0.,1.,0.));
#10999=DIRECTION('ref_axis',(1.,0.,0.));
#11000=DIRECTION('center_axis',(0.,1.,0.));
#11001=DIRECTION('ref_axis',(1.,0.,0.));
#11002=DIRECTION('',(0.,-1.,0.));
#11003=DIRECTION('center_axis',(0.,1.,0.));
#11004=DIRECTION('ref_axis',(1.,0.,0.));
#11005=DIRECTION('center_axis',(0.,1.,0.));
#11006=DIRECTION('ref_axis',(1.,0.,0.));
#11007=DIRECTION('center_axis',(0.,1.,0.));
#11008=DIRECTION('ref_axis',(1.,0.,0.));
#11009=DIRECTION('axis',(0.,0.,1.));
#11010=DIRECTION('refdir',(1.,0.,0.));
#11011=DIRECTION('center_axis',(-0.000134420183300025,-0.085636011539688,
0.996326480356107));
#11012=DIRECTION('ref_axis',(1.1553650826854E-5,-0.996326489423811,-0.0856360107603029));
#11013=DIRECTION('center_axis',(0.000134419999317792,-0.085636011399563,
0.996326480368176));
#11014=DIRECTION('ref_axis',(0.0962365814952688,0.991703136101715,0.0852256430197378));
#11015=DIRECTION('center_axis',(0.000134419999317792,-0.085636011399563,
0.996326480368176));
#11016=DIRECTION('ref_axis',(0.0962365814952688,0.991703136101715,0.0852256430197378));
#11017=DIRECTION('center_axis',(-0.000134420183300025,-0.085636011539688,
0.996326480356107));
#11018=DIRECTION('ref_axis',(1.1553650826854E-5,-0.996326489423811,-0.0856360107603029));
#11019=DIRECTION('axis',(0.,0.,1.));
#11020=DIRECTION('refdir',(1.,0.,0.));
#11021=DIRECTION('center_axis',(0.,1.,0.));
#11022=DIRECTION('ref_axis',(1.,0.,0.));
#11023=DIRECTION('center_axis',(0.,1.,0.));
#11024=DIRECTION('ref_axis',(1.,0.,0.));
#11025=DIRECTION('',(0.,-1.,0.));
#11026=DIRECTION('center_axis',(0.,1.,0.));
#11027=DIRECTION('ref_axis',(1.,0.,0.));
#11028=DIRECTION('center_axis',(0.,1.,0.));
#11029=DIRECTION('ref_axis',(1.,0.,0.));
#11030=DIRECTION('center_axis',(0.,1.,0.));
#11031=DIRECTION('ref_axis',(1.,0.,0.));
#11032=DIRECTION('axis',(0.,0.,1.));
#11033=DIRECTION('refdir',(1.,0.,0.));
#11034=DIRECTION('center_axis',(0.,1.,0.));
#11035=DIRECTION('ref_axis',(1.,0.,0.));
#11036=DIRECTION('center_axis',(0.,1.,0.));
#11037=DIRECTION('ref_axis',(1.,0.,0.));
#11038=DIRECTION('',(0.,-1.,0.));
#11039=DIRECTION('center_axis',(0.,1.,0.));
#11040=DIRECTION('ref_axis',(1.,0.,0.));
#11041=DIRECTION('center_axis',(0.,1.,0.));
#11042=DIRECTION('ref_axis',(1.,0.,0.));
#11043=DIRECTION('center_axis',(0.,1.,0.));
#11044=DIRECTION('ref_axis',(1.,0.,0.));
#11045=DIRECTION('axis',(0.,0.,1.));
#11046=DIRECTION('refdir',(1.,0.,0.));
#11047=DIRECTION('center_axis',(-0.000134420183300025,-0.085636011539688,
0.996326480356107));
#11048=DIRECTION('ref_axis',(1.1553650826854E-5,-0.996326489423811,-0.0856360107603029));
#11049=DIRECTION('center_axis',(0.000134419999317792,-0.085636011399563,
0.996326480368176));
#11050=DIRECTION('ref_axis',(0.0962365814952688,0.991703136101715,0.0852256430197378));
#11051=DIRECTION('center_axis',(0.000134419999317792,-0.085636011399563,
0.996326480368176));
#11052=DIRECTION('ref_axis',(0.0962365814952688,0.991703136101715,0.0852256430197378));
#11053=DIRECTION('center_axis',(-0.000134420183300025,-0.085636011539688,
0.996326480356107));
#11054=DIRECTION('ref_axis',(1.1553650826854E-5,-0.996326489423811,-0.0856360107603029));
#11055=DIRECTION('axis',(0.,0.,1.));
#11056=DIRECTION('refdir',(1.,0.,0.));
#11057=DIRECTION('center_axis',(0.,1.,0.));
#11058=DIRECTION('ref_axis',(0.,0.,1.));
#11059=DIRECTION('center_axis',(0.,-1.,0.));
#11060=DIRECTION('ref_axis',(1.,0.,0.));
#11061=DIRECTION('center_axis',(0.,-1.,0.));
#11062=DIRECTION('ref_axis',(1.,0.,0.));
#11063=DIRECTION('center_axis',(0.,-1.,0.));
#11064=DIRECTION('ref_axis',(1.,0.,0.));
#11065=DIRECTION('',(0.707106781186548,0.707106781186547,8.65956056235493E-17));
#11066=DIRECTION('center_axis',(0.,-1.,0.));
#11067=DIRECTION('ref_axis',(1.,0.,0.));
#11068=DIRECTION('center_axis',(0.,-1.,0.));
#11069=DIRECTION('ref_axis',(1.,0.,0.));
#11070=DIRECTION('',(0.,1.,0.));
#11071=DIRECTION('center_axis',(0.,1.,0.));
#11072=DIRECTION('ref_axis',(1.,0.,0.));
#11073=DIRECTION('center_axis',(0.,-1.,0.));
#11074=DIRECTION('ref_axis',(1.,0.,0.));
#11075=DIRECTION('',(-0.707106781186547,0.707106781186548,-8.65956056235493E-17));
#11076=DIRECTION('center_axis',(0.,-1.,0.));
#11077=DIRECTION('ref_axis',(0.,0.,-1.));
#11078=DIRECTION('center_axis',(0.,-1.,0.));
#11079=DIRECTION('ref_axis',(1.,0.,0.));
#11080=DIRECTION('center_axis',(0.,1.,0.));
#11081=DIRECTION('ref_axis',(1.,0.,0.));
#11082=DIRECTION('center_axis',(0.,1.,0.));
#11083=DIRECTION('ref_axis',(1.,0.,0.));
#11084=DIRECTION('',(-0.447213595499958,0.894427190999916,-5.47678698264203E-17));
#11085=DIRECTION('center_axis',(0.,-1.,0.));
#11086=DIRECTION('ref_axis',(1.,0.,0.));
#11087=DIRECTION('center_axis',(0.,1.,0.));
#11088=DIRECTION('ref_axis',(1.,0.,0.));
#11089=DIRECTION('',(0.,1.,0.));
#11090=DIRECTION('center_axis',(0.,1.,0.));
#11091=DIRECTION('ref_axis',(1.,0.,0.));
#11092=DIRECTION('center_axis',(0.,-1.,0.));
#11093=DIRECTION('ref_axis',(1.,0.,0.));
#11094=DIRECTION('',(-0.707106781186547,0.707106781186548,-8.65956056235493E-17));
#11095=DIRECTION('center_axis',(0.,-1.,0.));
#11096=DIRECTION('ref_axis',(0.,0.,-1.));
#11097=DIRECTION('center_axis',(0.866025403784439,0.,-0.5));
#11098=DIRECTION('ref_axis',(0.5,0.,0.866025403784439));
#11099=DIRECTION('',(-0.5,0.,-0.866025403784439));
#11100=DIRECTION('',(0.,-1.,0.));
#11101=DIRECTION('',(0.5,0.,0.866025403784439));
#11102=DIRECTION('',(0.,-1.,0.));
#11103=DIRECTION('center_axis',(1.20185167898973E-16,0.,-1.));
#11104=DIRECTION('ref_axis',(1.,0.,1.20185167898973E-16));
#11105=DIRECTION('',(-1.,0.,-1.20185167898973E-16));
#11106=DIRECTION('',(0.,-1.,0.));
#11107=DIRECTION('',(1.,0.,1.20185167898973E-16));
#11108=DIRECTION('center_axis',(-0.866025403784439,0.,-0.5));
#11109=DIRECTION('ref_axis',(0.5,0.,-0.866025403784439));
#11110=DIRECTION('',(-0.5,0.,0.866025403784439));
#11111=DIRECTION('',(0.,-1.,0.));
#11112=DIRECTION('',(0.5,0.,-0.866025403784439));
#11113=DIRECTION('center_axis',(-0.866025403784439,0.,0.5));
#11114=DIRECTION('ref_axis',(-0.5,0.,-0.866025403784439));
#11115=DIRECTION('',(0.5,0.,0.866025403784439));
#11116=DIRECTION('',(0.,-1.,0.));
#11117=DIRECTION('',(-0.5,0.,-0.866025403784439));
#11118=DIRECTION('center_axis',(-2.40370335797945E-16,0.,1.));
#11119=DIRECTION('ref_axis',(-1.,0.,-2.40370335797945E-16));
#11120=DIRECTION('',(1.,0.,2.40370335797945E-16));
#11121=DIRECTION('',(0.,-1.,0.));
#11122=DIRECTION('',(-1.,0.,-2.40370335797945E-16));
#11123=DIRECTION('center_axis',(0.866025403784439,0.,0.5));
#11124=DIRECTION('ref_axis',(-0.5,0.,0.866025403784439));
#11125=DIRECTION('',(0.5,0.,-0.866025403784439));
#11126=DIRECTION('',(-0.5,0.,0.866025403784439));
#11127=DIRECTION('center_axis',(0.,1.,0.));
#11128=DIRECTION('ref_axis',(1.,0.,0.));
#11129=DIRECTION('center_axis',(0.,-1.,0.));
#11130=DIRECTION('ref_axis',(0.,0.,-1.));
#11131=DIRECTION('axis',(0.,0.,1.));
#11132=DIRECTION('refdir',(1.,0.,0.));
#11133=DIRECTION('axis',(0.,0.,1.));
#11134=DIRECTION('refdir',(1.,0.,0.));
#11135=DIRECTION('center_axis',(0.,-1.,0.));
#11136=DIRECTION('ref_axis',(0.,0.,-1.));
#11137=DIRECTION('center_axis',(0.,-1.,0.));
#11138=DIRECTION('ref_axis',(1.,0.,0.));
#11139=DIRECTION('center_axis',(0.,-1.,0.));
#11140=DIRECTION('ref_axis',(1.,0.,0.));
#11141=DIRECTION('center_axis',(1.,0.,1.22464679914735E-16));
#11142=DIRECTION('ref_axis',(-1.22464679914735E-16,0.,1.));
#11143=DIRECTION('center_axis',(0.,1.,0.));
#11144=DIRECTION('ref_axis',(1.,0.,0.));
#11145=DIRECTION('center_axis',(0.,1.,0.));
#11146=DIRECTION('ref_axis',(1.,0.,0.));
#11147=DIRECTION('center_axis',(0.,-1.,0.));
#11148=DIRECTION('ref_axis',(1.,0.,0.));
#11149=DIRECTION('',(0.,1.,0.));
#11150=DIRECTION('center_axis',(0.,-1.,0.));
#11151=DIRECTION('ref_axis',(1.,0.,0.));
#11152=DIRECTION('center_axis',(0.,-1.,0.));
#11153=DIRECTION('ref_axis',(1.,0.,0.));
#11154=DIRECTION('center_axis',(0.,-1.,0.));
#11155=DIRECTION('ref_axis',(1.,0.,0.));
#11156=DIRECTION('',(0.,1.,0.));
#11157=DIRECTION('center_axis',(0.,-1.,0.));
#11158=DIRECTION('ref_axis',(1.,0.,0.));
#11159=DIRECTION('center_axis',(0.,1.,0.));
#11160=DIRECTION('ref_axis',(1.,0.,0.));
#11161=DIRECTION('',(-0.707106781186548,0.707106781186547,-8.65956056235493E-17));
#11162=DIRECTION('center_axis',(0.,-1.,0.));
#11163=DIRECTION('ref_axis',(1.,0.,0.));
#11164=DIRECTION('center_axis',(0.,1.,0.));
#11165=DIRECTION('ref_axis',(0.,0.,1.));
#11166=DIRECTION('center_axis',(0.,-1.,0.));
#11167=DIRECTION('ref_axis',(1.,0.,0.));
#11168=DIRECTION('center_axis',(0.,-1.,0.));
#11169=DIRECTION('ref_axis',(1.,0.,0.));
#11170=DIRECTION('',(0.,1.,0.));
#11171=DIRECTION('center_axis',(0.,-1.,0.));
#11172=DIRECTION('ref_axis',(0.,0.,-1.));
#11173=DIRECTION('center_axis',(0.,-1.,0.));
#11174=DIRECTION('ref_axis',(1.,0.,0.));
#11175=DIRECTION('center_axis',(0.,-1.,0.));
#11176=DIRECTION('ref_axis',(1.,0.,0.));
#11177=DIRECTION('',(0.707106781186548,0.707106781186547,8.65956056235493E-17));
#11178=DIRECTION('axis',(0.,0.,1.));
#11179=DIRECTION('refdir',(1.,0.,0.));
#11180=DIRECTION('center_axis',(0.,-1.,0.));
#11181=DIRECTION('ref_axis',(0.,0.,-1.));
#11182=DIRECTION('center_axis',(0.,-1.,0.));
#11183=DIRECTION('ref_axis',(1.,0.,0.));
#11184=DIRECTION('center_axis',(0.,-1.,0.));
#11185=DIRECTION('ref_axis',(1.,0.,0.));
#11186=DIRECTION('center_axis',(1.,0.,1.22464679914735E-16));
#11187=DIRECTION('ref_axis',(-1.22464679914735E-16,0.,1.));
#11188=DIRECTION('center_axis',(0.,1.,0.));
#11189=DIRECTION('ref_axis',(1.,0.,0.));
#11190=DIRECTION('center_axis',(0.,1.,0.));
#11191=DIRECTION('ref_axis',(1.,0.,0.));
#11192=DIRECTION('center_axis',(0.,-1.,0.));
#11193=DIRECTION('ref_axis',(1.,0.,0.));
#11194=DIRECTION('center_axis',(0.,-1.,0.));
#11195=DIRECTION('ref_axis',(1.,0.,0.));
#11196=DIRECTION('',(0.,1.,0.));
#11197=DIRECTION('center_axis',(0.,1.,0.));
#11198=DIRECTION('ref_axis',(0.,0.,1.));
#11199=DIRECTION('center_axis',(0.,-1.,0.));
#11200=DIRECTION('ref_axis',(1.,0.,0.));
#11201=DIRECTION('center_axis',(0.,-1.,0.));
#11202=DIRECTION('ref_axis',(1.,0.,0.));
#11203=DIRECTION('center_axis',(0.,-1.,0.));
#11204=DIRECTION('ref_axis',(1.,0.,0.));
#11205=DIRECTION('center_axis',(0.,-1.,0.));
#11206=DIRECTION('ref_axis',(1.,0.,0.));
#11207=DIRECTION('',(0.707106781186548,0.707106781186547,8.65956056235494E-17));
#11208=DIRECTION('center_axis',(0.,-1.,0.));
#11209=DIRECTION('ref_axis',(1.,0.,0.));
#11210=DIRECTION('center_axis',(0.,-1.,0.));
#11211=DIRECTION('ref_axis',(1.,0.,0.));
#11212=DIRECTION('',(0.,1.,0.));
#11213=DIRECTION('center_axis',(0.,1.,0.));
#11214=DIRECTION('ref_axis',(1.,0.,0.));
#11215=DIRECTION('center_axis',(0.,-1.,0.));
#11216=DIRECTION('ref_axis',(1.,0.,0.));
#11217=DIRECTION('',(-0.707106781186548,0.707106781186547,-8.65956056235494E-17));
#11218=DIRECTION('center_axis',(0.,-1.,0.));
#11219=DIRECTION('ref_axis',(0.,0.,-1.));
#11220=DIRECTION('center_axis',(0.,-1.,0.));
#11221=DIRECTION('ref_axis',(1.,0.,0.));
#11222=DIRECTION('',(0.,1.,0.));
#11223=DIRECTION('axis',(0.,0.,1.));
#11224=DIRECTION('refdir',(1.,0.,0.));
#11225=DIRECTION('center_axis',(0.,0.,1.));
#11226=DIRECTION('ref_axis',(1.,0.,0.));
#11227=DIRECTION('center_axis',(1.22464679914735E-16,-1.,0.));
#11228=DIRECTION('ref_axis',(-1.,-1.22464679914735E-16,0.));
#11229=DIRECTION('center_axis',(0.78183148246803,0.,0.623489801858733));
#11230=DIRECTION('ref_axis',(0.623489801858734,0.,-0.78183148246803));
#11231=DIRECTION('center_axis',(7.63554790147315E-17,-1.,-9.57467422477103E-17));
#11232=DIRECTION('ref_axis',(-0.623489801858734,-1.22464679914735E-16,0.78183148246803));
#11233=DIRECTION('center_axis',(0.974927912181824,0.,-0.222520933956314));
#11234=DIRECTION('ref_axis',(-0.222520933956314,0.,-0.974927912181824));
#11235=DIRECTION('center_axis',(-2.7250954951288E-17,-1.,-1.19394234705288E-16));
#11236=DIRECTION('ref_axis',(0.222520933956314,-1.22464679914735E-16,0.974927912181824));
#11237=DIRECTION('center_axis',(0.433883739117558,0.,-0.900968867902419));
#11238=DIRECTION('ref_axis',(-0.900968867902419,0.,-0.433883739117558));
#11239=DIRECTION('center_axis',(-1.10336864020811E-16,-1.,-5.31354332312403E-17));
#11240=DIRECTION('ref_axis',(0.900968867902419,-1.22464679914735E-16,0.433883739117558));
#11241=DIRECTION('center_axis',(-0.433883739117558,0.,-0.900968867902419));
#11242=DIRECTION('ref_axis',(-0.900968867902419,0.,0.433883739117558));
#11243=DIRECTION('center_axis',(-1.10336864020811E-16,-1.,5.31354332312403E-17));
#11244=DIRECTION('ref_axis',(0.900968867902419,-1.22464679914735E-16,-0.433883739117558));
#11245=DIRECTION('center_axis',(-0.974927912181824,0.,-0.222520933956314));
#11246=DIRECTION('ref_axis',(-0.222520933956315,0.,0.974927912181824));
#11247=DIRECTION('center_axis',(-2.7250954951288E-17,-1.,1.19394234705288E-16));
#11248=DIRECTION('ref_axis',(0.222520933956315,-1.22464679914735E-16,-0.974927912181824));
#11249=DIRECTION('center_axis',(-0.78183148246803,0.,0.623489801858734));
#11250=DIRECTION('ref_axis',(0.623489801858733,0.,0.78183148246803));
#11251=DIRECTION('center_axis',(7.63554790147315E-17,-1.,9.57467422477103E-17));
#11252=DIRECTION('ref_axis',(-0.623489801858733,-1.22464679914735E-16,-0.78183148246803));
#11253=DIRECTION('axis',(0.,0.,1.));
#11254=DIRECTION('refdir',(1.,0.,0.));
#11255=DIRECTION('center_axis',(0.,0.,1.));
#11256=DIRECTION('ref_axis',(1.,0.,0.));
#11257=DIRECTION('center_axis',(0.,-1.,0.));
#11258=DIRECTION('ref_axis',(0.,0.,-1.));
#11259=DIRECTION('center_axis',(0.,-1.,0.));
#11260=DIRECTION('ref_axis',(0.,0.,-1.));
#11261=DIRECTION('center_axis',(0.,1.,0.));
#11262=DIRECTION('ref_axis',(1.,0.,0.));
#11263=DIRECTION('center_axis',(0.,1.,0.));
#11264=DIRECTION('ref_axis',(1.,0.,0.));
#11265=DIRECTION('center_axis',(0.,1.,0.));
#11266=DIRECTION('ref_axis',(1.,0.,0.));
#11267=DIRECTION('center_axis',(0.,1.,0.));
#11268=DIRECTION('ref_axis',(1.,0.,0.));
#11269=DIRECTION('',(0.,-1.,0.));
#11270=DIRECTION('center_axis',(0.,-1.,0.));
#11271=DIRECTION('ref_axis',(1.,0.,0.));
#11272=DIRECTION('center_axis',(0.,1.,0.));
#11273=DIRECTION('ref_axis',(1.,0.,0.));
#11274=DIRECTION('center_axis',(0.,1.,0.));
#11275=DIRECTION('ref_axis',(1.,0.,0.));
#11276=DIRECTION('center_axis',(0.,1.,0.));
#11277=DIRECTION('ref_axis',(1.,0.,0.));
#11278=DIRECTION('center_axis',(0.,1.,0.));
#11279=DIRECTION('ref_axis',(1.,0.,0.));
#11280=DIRECTION('center_axis',(0.,1.,0.));
#11281=DIRECTION('ref_axis',(1.,0.,0.));
#11282=DIRECTION('center_axis',(0.,1.,0.));
#11283=DIRECTION('ref_axis',(1.,0.,0.));
#11284=DIRECTION('center_axis',(0.,-1.,0.));
#11285=DIRECTION('ref_axis',(1.,0.,0.));
#11286=DIRECTION('center_axis',(0.,-1.,0.));
#11287=DIRECTION('ref_axis',(0.,0.,-1.));
#11288=DIRECTION('center_axis',(8.96625347776458E-17,0.,1.));
#11289=DIRECTION('ref_axis',(1.,0.,0.));
#11290=DIRECTION('center_axis',(0.,-1.,0.));
#11291=DIRECTION('ref_axis',(0.,0.,-1.));
#11292=DIRECTION('center_axis',(0.,1.,0.));
#11293=DIRECTION('ref_axis',(1.,0.,0.));
#11294=DIRECTION('center_axis',(0.,-1.,0.));
#11295=DIRECTION('ref_axis',(1.,0.,0.));
#11296=DIRECTION('center_axis',(0.,-1.,0.));
#11297=DIRECTION('ref_axis',(0.,0.,-1.));
#11298=DIRECTION('center_axis',(0.,0.,1.));
#11299=DIRECTION('ref_axis',(1.,0.,0.));
#11300=DIRECTION('center_axis',(0.,-1.,0.));
#11301=DIRECTION('ref_axis',(0.,0.,-1.));
#11302=DIRECTION('center_axis',(0.,1.,0.));
#11303=DIRECTION('ref_axis',(1.,0.,0.));
#11304=DIRECTION('center_axis',(0.,-1.,0.));
#11305=DIRECTION('ref_axis',(1.,0.,0.));
#11306=DIRECTION('center_axis',(0.,-1.,0.));
#11307=DIRECTION('ref_axis',(1.,0.,0.));
#11308=DIRECTION('center_axis',(0.,-1.,0.));
#11309=DIRECTION('ref_axis',(0.,0.,-1.));
#11310=DIRECTION('center_axis',(0.,0.,1.));
#11311=DIRECTION('ref_axis',(1.,0.,0.));
#11312=DIRECTION('center_axis',(0.,-1.,0.));
#11313=DIRECTION('ref_axis',(0.,0.,-1.));
#11314=DIRECTION('center_axis',(0.,1.,0.));
#11315=DIRECTION('ref_axis',(1.,0.,0.));
#11316=DIRECTION('center_axis',(0.,-1.,0.));
#11317=DIRECTION('ref_axis',(1.,0.,0.));
#11318=DIRECTION('center_axis',(0.,-1.,0.));
#11319=DIRECTION('ref_axis',(0.,0.,-1.));
#11320=DIRECTION('center_axis',(8.96625347776458E-17,0.,1.));
#11321=DIRECTION('ref_axis',(1.,0.,0.));
#11322=DIRECTION('center_axis',(0.,-1.,0.));
#11323=DIRECTION('ref_axis',(0.,0.,-1.));
#11324=DIRECTION('center_axis',(0.,1.,0.));
#11325=DIRECTION('ref_axis',(1.,0.,0.));
#11326=DIRECTION('center_axis',(0.,-1.,0.));
#11327=DIRECTION('ref_axis',(1.,0.,0.));
#11328=DIRECTION('center_axis',(0.,-1.,0.));
#11329=DIRECTION('ref_axis',(0.,0.,-1.));
#11330=DIRECTION('center_axis',(0.,0.,1.));
#11331=DIRECTION('ref_axis',(1.,0.,0.));
#11332=DIRECTION('center_axis',(0.,-1.,0.));
#11333=DIRECTION('ref_axis',(0.,0.,-1.));
#11334=DIRECTION('center_axis',(0.,1.,0.));
#11335=DIRECTION('ref_axis',(1.,0.,0.));
#11336=DIRECTION('center_axis',(0.,1.,0.));
#11337=DIRECTION('ref_axis',(1.,0.,0.));
#11338=DIRECTION('',(0.,1.,0.));
#11339=DIRECTION('center_axis',(0.,-1.,0.));
#11340=DIRECTION('ref_axis',(1.,0.,0.));
#11341=DIRECTION('center_axis',(0.,-1.,0.));
#11342=DIRECTION('ref_axis',(1.,0.,0.));
#11343=DIRECTION('center_axis',(0.,1.,0.));
#11344=DIRECTION('ref_axis',(1.,0.,0.));
#11345=DIRECTION('center_axis',(0.,-1.,0.));
#11346=DIRECTION('ref_axis',(0.,0.,-1.));
#11347=DIRECTION('center_axis',(0.,0.,1.));
#11348=DIRECTION('ref_axis',(1.,0.,0.));
#11349=DIRECTION('center_axis',(0.,-1.,0.));
#11350=DIRECTION('ref_axis',(0.,0.,-1.));
#11351=DIRECTION('center_axis',(0.,-1.,0.));
#11352=DIRECTION('ref_axis',(-1.,0.,0.));
#11353=DIRECTION('center_axis',(0.,1.,0.));
#11354=DIRECTION('ref_axis',(1.,0.,0.));
#11355=DIRECTION('axis',(0.,0.,1.));
#11356=DIRECTION('refdir',(1.,0.,0.));
#11357=DIRECTION('center_axis',(0.,1.,0.));
#11358=DIRECTION('ref_axis',(0.,0.,1.));
#11359=DIRECTION('center_axis',(0.,-1.,0.));
#11360=DIRECTION('ref_axis',(1.,0.,0.));
#11361=DIRECTION('center_axis',(0.,-1.,0.));
#11362=DIRECTION('ref_axis',(1.,0.,0.));
#11363=DIRECTION('center_axis',(0.,-1.,0.));
#11364=DIRECTION('ref_axis',(1.,0.,0.));
#11365=DIRECTION('center_axis',(0.,-1.,0.));
#11366=DIRECTION('ref_axis',(1.,0.,0.));
#11367=DIRECTION('',(0.,1.,0.));
#11368=DIRECTION('center_axis',(0.,-1.,0.));
#11369=DIRECTION('ref_axis',(0.,0.,-1.));
#11370=DIRECTION('center_axis',(0.,-1.,0.));
#11371=DIRECTION('ref_axis',(1.,0.,0.));
#11372=DIRECTION('center_axis',(0.,-1.,0.));
#11373=DIRECTION('ref_axis',(1.,0.,0.));
#11374=DIRECTION('',(0.,1.,0.));
#11375=DIRECTION('center_axis',(0.,1.,0.));
#11376=DIRECTION('ref_axis',(0.,0.,1.));
#11377=DIRECTION('center_axis',(0.,-1.,0.));
#11378=DIRECTION('ref_axis',(1.,0.,0.));
#11379=DIRECTION('center_axis',(0.,-1.,0.));
#11380=DIRECTION('ref_axis',(1.,0.,0.));
#11381=DIRECTION('center_axis',(0.,-1.,0.));
#11382=DIRECTION('ref_axis',(1.,0.,0.));
#11383=DIRECTION('center_axis',(0.,-1.,0.));
#11384=DIRECTION('ref_axis',(1.,0.,0.));
#11385=DIRECTION('',(0.,1.,0.));
#11386=DIRECTION('center_axis',(0.,-1.,0.));
#11387=DIRECTION('ref_axis',(0.,0.,-1.));
#11388=DIRECTION('center_axis',(0.,-1.,0.));
#11389=DIRECTION('ref_axis',(1.,0.,0.));
#11390=DIRECTION('center_axis',(0.,-1.,0.));
#11391=DIRECTION('ref_axis',(1.,0.,0.));
#11392=DIRECTION('',(0.,1.,0.));
#11393=DIRECTION('',(0.,0.,1.));
#11394=DIRECTION('',(1.,0.,0.));
#11395=DIRECTION('',(0.,0.,1.));
#11396=DIRECTION('',(1.,0.,0.));
#11397=DIRECTION('',(0.,0.,1.));
#11398=DIRECTION('',(1.,0.,0.));
#11399=DIRECTION('',(0.,0.,1.));
#11400=DIRECTION('',(1.,0.,0.));
#11401=DIRECTION('',(0.,0.,1.));
#11402=DIRECTION('',(1.,0.,0.));
#11403=DIRECTION('axis',(0.,0.,1.));
#11404=DIRECTION('refdir',(1.,0.,0.));
#11405=DIRECTION('center_axis',(0.866025403784439,0.,-0.5));
#11406=DIRECTION('ref_axis',(0.5,0.,0.866025403784439));
#11407=DIRECTION('',(-0.5,0.,-0.866025403784439));
#11408=DIRECTION('',(0.,-1.,0.));
#11409=DIRECTION('',(0.5,0.,0.866025403784439));
#11410=DIRECTION('',(0.,-1.,0.));
#11411=DIRECTION('center_axis',(1.60246890531964E-16,0.,-1.));
#11412=DIRECTION('ref_axis',(1.,0.,1.60246890531964E-16));
#11413=DIRECTION('',(-1.,0.,-1.60246890531964E-16));
#11414=DIRECTION('',(0.,-1.,0.));
#11415=DIRECTION('',(1.,0.,1.60246890531964E-16));
#11416=DIRECTION('center_axis',(-0.866025403784439,0.,-0.5));
#11417=DIRECTION('ref_axis',(0.5,0.,-0.866025403784439));
#11418=DIRECTION('',(-0.5,0.,0.866025403784439));
#11419=DIRECTION('',(0.,-1.,0.));
#11420=DIRECTION('',(0.5,0.,-0.866025403784439));
#11421=DIRECTION('center_axis',(-0.866025403784439,0.,0.5));
#11422=DIRECTION('ref_axis',(-0.5,0.,-0.866025403784439));
#11423=DIRECTION('',(0.5,0.,0.866025403784439));
#11424=DIRECTION('',(0.,-1.,0.));
#11425=DIRECTION('',(-0.5,0.,-0.866025403784439));
#11426=DIRECTION('center_axis',(-1.60246890531964E-16,0.,1.));
#11427=DIRECTION('ref_axis',(-1.,0.,-1.60246890531964E-16));
#11428=DIRECTION('',(1.,0.,1.60246890531964E-16));
#11429=DIRECTION('',(0.,-1.,0.));
#11430=DIRECTION('',(-1.,0.,-1.60246890531964E-16));
#11431=DIRECTION('center_axis',(0.866025403784439,0.,0.5));
#11432=DIRECTION('ref_axis',(-0.5,0.,0.866025403784439));
#11433=DIRECTION('',(0.5,0.,-0.866025403784439));
#11434=DIRECTION('',(-0.5,0.,0.866025403784439));
#11435=DIRECTION('center_axis',(0.,1.,0.));
#11436=DIRECTION('ref_axis',(1.,0.,0.));
#11437=DIRECTION('center_axis',(0.,-1.,0.));
#11438=DIRECTION('ref_axis',(0.,0.,-1.));
#11439=DIRECTION('center_axis',(0.,1.,0.));
#11440=DIRECTION('ref_axis',(1.,0.,0.));
#11441=DIRECTION('center_axis',(0.,1.,0.));
#11442=DIRECTION('ref_axis',(1.,0.,0.));
#11443=DIRECTION('center_axis',(0.,1.,0.));
#11444=DIRECTION('ref_axis',(0.,0.,1.));
#11445=DIRECTION('center_axis',(0.,-1.,0.));
#11446=DIRECTION('ref_axis',(1.,0.,0.));
#11447=DIRECTION('center_axis',(0.,-1.,0.));
#11448=DIRECTION('ref_axis',(1.,0.,0.));
#11449=DIRECTION('center_axis',(0.,-1.,0.));
#11450=DIRECTION('ref_axis',(1.,0.,0.));
#11451=DIRECTION('',(0.707106781186547,0.707106781186548,8.65956056235493E-17));
#11452=DIRECTION('center_axis',(0.,-1.,0.));
#11453=DIRECTION('ref_axis',(1.,0.,0.));
#11454=DIRECTION('center_axis',(0.,-1.,0.));
#11455=DIRECTION('ref_axis',(1.,0.,0.));
#11456=DIRECTION('',(0.,1.,0.));
#11457=DIRECTION('center_axis',(0.,1.,0.));
#11458=DIRECTION('ref_axis',(1.,0.,0.));
#11459=DIRECTION('center_axis',(0.,-1.,0.));
#11460=DIRECTION('ref_axis',(1.,0.,0.));
#11461=DIRECTION('',(-0.707106781186547,0.707106781186548,-8.65956056235493E-17));
#11462=DIRECTION('center_axis',(0.,-1.,0.));
#11463=DIRECTION('ref_axis',(0.,0.,-1.));
#11464=DIRECTION('center_axis',(0.,-1.,0.));
#11465=DIRECTION('ref_axis',(1.,0.,0.));
#11466=DIRECTION('center_axis',(0.,1.,0.));
#11467=DIRECTION('ref_axis',(1.,0.,0.));
#11468=DIRECTION('center_axis',(0.,1.,0.));
#11469=DIRECTION('ref_axis',(1.,0.,0.));
#11470=DIRECTION('',(-0.447213595499958,0.894427190999916,-5.47678698264203E-17));
#11471=DIRECTION('center_axis',(0.,-1.,0.));
#11472=DIRECTION('ref_axis',(1.,0.,0.));
#11473=DIRECTION('',(0.,1.,0.));
#11474=DIRECTION('axis',(0.,0.,1.));
#11475=DIRECTION('refdir',(1.,0.,0.));
#11476=DIRECTION('center_axis',(0.,1.,0.));
#11477=DIRECTION('ref_axis',(0.,0.,1.));
#11478=DIRECTION('center_axis',(0.,-1.,0.));
#11479=DIRECTION('ref_axis',(1.,0.,0.));
#11480=DIRECTION('center_axis',(0.,-1.,0.));
#11481=DIRECTION('ref_axis',(1.,0.,0.));
#11482=DIRECTION('center_axis',(0.,-1.,0.));
#11483=DIRECTION('ref_axis',(1.,0.,0.));
#11484=DIRECTION('',(0.707106781186548,0.707106781186547,8.65956056235494E-17));
#11485=DIRECTION('center_axis',(0.,-1.,0.));
#11486=DIRECTION('ref_axis',(1.,0.,0.));
#11487=DIRECTION('center_axis',(0.,-1.,0.));
#11488=DIRECTION('ref_axis',(1.,0.,0.));
#11489=DIRECTION('',(0.,1.,0.));
#11490=DIRECTION('center_axis',(0.,1.,0.));
#11491=DIRECTION('ref_axis',(1.,0.,0.));
#11492=DIRECTION('center_axis',(0.,-1.,0.));
#11493=DIRECTION('ref_axis',(1.,0.,0.));
#11494=DIRECTION('',(-0.707106781186547,0.707106781186548,-8.65956056235493E-17));
#11495=DIRECTION('center_axis',(0.,-1.,0.));
#11496=DIRECTION('ref_axis',(0.,0.,-1.));
#11497=DIRECTION('center_axis',(0.,-1.,0.));
#11498=DIRECTION('ref_axis',(1.,0.,0.));
#11499=DIRECTION('center_axis',(0.,1.,0.));
#11500=DIRECTION('ref_axis',(1.,0.,0.));
#11501=DIRECTION('center_axis',(0.,1.,0.));
#11502=DIRECTION('ref_axis',(1.,0.,0.));
#11503=DIRECTION('',(-0.447213595499958,0.894427190999916,-5.47678698264203E-17));
#11504=DIRECTION('center_axis',(0.,-1.,0.));
#11505=DIRECTION('ref_axis',(1.,0.,0.));
#11506=DIRECTION('center_axis',(0.,1.,0.));
#11507=DIRECTION('ref_axis',(1.,0.,0.));
#11508=DIRECTION('',(0.,1.,0.));
#11509=DIRECTION('center_axis',(0.,1.,0.));
#11510=DIRECTION('ref_axis',(1.,0.,0.));
#11511=DIRECTION('center_axis',(0.,-1.,0.));
#11512=DIRECTION('ref_axis',(1.,0.,0.));
#11513=DIRECTION('',(-0.707106781186547,0.707106781186548,-8.65956056235493E-17));
#11514=DIRECTION('center_axis',(0.,-1.,0.));
#11515=DIRECTION('ref_axis',(0.,0.,-1.));
#11516=DIRECTION('center_axis',(0.866025403784439,0.,-0.5));
#11517=DIRECTION('ref_axis',(0.5,0.,0.866025403784439));
#11518=DIRECTION('',(-0.5,0.,-0.866025403784439));
#11519=DIRECTION('',(0.,-1.,0.));
#11520=DIRECTION('',(0.5,0.,0.866025403784439));
#11521=DIRECTION('',(0.,-1.,0.));
#11522=DIRECTION('center_axis',(1.92296268638356E-16,0.,-1.));
#11523=DIRECTION('ref_axis',(1.,0.,1.92296268638356E-16));
#11524=DIRECTION('',(-1.,0.,-1.92296268638356E-16));
#11525=DIRECTION('',(0.,-1.,0.));
#11526=DIRECTION('',(1.,0.,1.92296268638356E-16));
#11527=DIRECTION('center_axis',(-0.866025403784439,0.,-0.5));
#11528=DIRECTION('ref_axis',(0.5,0.,-0.866025403784439));
#11529=DIRECTION('',(-0.5,0.,0.866025403784438));
#11530=DIRECTION('',(0.,-1.,0.));
#11531=DIRECTION('',(0.5,0.,-0.866025403784438));
#11532=DIRECTION('center_axis',(-0.866025403784439,0.,0.5));
#11533=DIRECTION('ref_axis',(-0.5,0.,-0.866025403784439));
#11534=DIRECTION('',(0.5,0.,0.866025403784439));
#11535=DIRECTION('',(0.,-1.,0.));
#11536=DIRECTION('',(-0.5,0.,-0.866025403784439));
#11537=DIRECTION('center_axis',(-1.92296268638356E-16,0.,1.));
#11538=DIRECTION('ref_axis',(-1.,0.,-1.92296268638356E-16));
#11539=DIRECTION('',(1.,0.,1.92296268638356E-16));
#11540=DIRECTION('',(0.,-1.,0.));
#11541=DIRECTION('',(-1.,0.,-1.92296268638356E-16));
#11542=DIRECTION('center_axis',(0.866025403784439,0.,0.5));
#11543=DIRECTION('ref_axis',(-0.5,0.,0.866025403784439));
#11544=DIRECTION('',(0.5,0.,-0.866025403784439));
#11545=DIRECTION('',(-0.5,0.,0.866025403784439));
#11546=DIRECTION('center_axis',(0.,1.,0.));
#11547=DIRECTION('ref_axis',(1.,0.,0.));
#11548=DIRECTION('center_axis',(0.,-1.,0.));
#11549=DIRECTION('ref_axis',(0.,0.,-1.));
#11550=DIRECTION('axis',(0.,0.,1.));
#11551=DIRECTION('refdir',(1.,0.,0.));
#11552=DIRECTION('center_axis',(0.,1.,0.));
#11553=DIRECTION('ref_axis',(1.,0.,0.));
#11554=DIRECTION('',(0.866025403784439,-0.5,1.06057523872491E-16));
#11555=DIRECTION('center_axis',(0.,-1.,0.));
#11556=DIRECTION('ref_axis',(1.,0.,0.));
#11557=DIRECTION('center_axis',(0.,-1.,0.));
#11558=DIRECTION('ref_axis',(1.,0.,0.));
#11559=DIRECTION('center_axis',(0.,1.,0.));
#11560=DIRECTION('ref_axis',(1.,0.,0.));
#11561=DIRECTION('',(-0.866025403784439,-0.5,-1.06057523872491E-16));
#11562=DIRECTION('center_axis',(1.92296268638356E-16,0.,-1.));
#11563=DIRECTION('ref_axis',(-1.,0.,-1.92296268638356E-16));
#11564=DIRECTION('',(0.,1.,0.));
#11565=DIRECTION('',(0.,1.,0.));
#11566=DIRECTION('center_axis',(-0.866025403784439,0.,-0.5));
#11567=DIRECTION('ref_axis',(-0.5,0.,0.866025403784439));
#11568=DIRECTION('',(0.,1.,0.));
#11569=DIRECTION('center_axis',(-0.866025403784439,0.,0.5));
#11570=DIRECTION('ref_axis',(0.5,0.,0.866025403784439));
#11571=DIRECTION('',(0.,1.,0.));
#11572=DIRECTION('center_axis',(0.,1.,0.));
#11573=DIRECTION('ref_axis',(1.,0.,0.));
#11574=DIRECTION('center_axis',(0.,1.,0.));
#11575=DIRECTION('ref_axis',(1.,0.,0.));
#11576=DIRECTION('',(0.,-1.,0.));
#11577=DIRECTION('center_axis',(0.,1.,0.));
#11578=DIRECTION('ref_axis',(1.,0.,0.));
#11579=DIRECTION('center_axis',(-1.92296268638356E-16,0.,1.));
#11580=DIRECTION('ref_axis',(1.,0.,1.92296268638356E-16));
#11581=DIRECTION('',(0.,1.,0.));
#11582=DIRECTION('center_axis',(0.866025403784439,0.,-0.5));
#11583=DIRECTION('ref_axis',(-0.5,0.,-0.866025403784439));
#11584=DIRECTION('',(0.,1.,0.));
#11585=DIRECTION('center_axis',(0.866025403784439,0.,0.5));
#11586=DIRECTION('ref_axis',(0.5,0.,-0.866025403784439));
#11587=DIRECTION('center_axis',(0.,1.,0.));
#11588=DIRECTION('ref_axis',(1.,0.,0.));
#11589=DIRECTION('center_axis',(0.,1.,0.));
#11590=DIRECTION('ref_axis',(1.,0.,0.));
#11591=DIRECTION('axis',(0.,0.,1.));
#11592=DIRECTION('refdir',(1.,0.,0.));
#11593=DIRECTION('axis',(0.,0.,1.));
#11594=DIRECTION('refdir',(1.,0.,0.));
#11595=DIRECTION('center_axis',(0.,1.,0.));
#11596=DIRECTION('ref_axis',(1.,0.,0.));
#11597=DIRECTION('center_axis',(0.,1.,0.));
#11598=DIRECTION('ref_axis',(1.,0.,0.));
#11599=DIRECTION('',(0.,1.,0.));
#11600=DIRECTION('center_axis',(0.,-1.,0.));
#11601=DIRECTION('ref_axis',(1.,0.,0.));
#11602=DIRECTION('center_axis',(0.,1.,0.));
#11603=DIRECTION('ref_axis',(1.,0.,0.));
#11604=DIRECTION('center_axis',(-1.,0.,0.));
#11605=DIRECTION('ref_axis',(0.,0.,1.));
#11606=DIRECTION('',(0.,-1.,0.));
#11607=DIRECTION('',(0.,0.,1.));
#11608=DIRECTION('',(0.,1.,0.));
#11609=DIRECTION('',(0.,0.,-1.));
#11610=DIRECTION('center_axis',(0.,1.,0.));
#11611=DIRECTION('ref_axis',(1.,0.,0.));
#11612=DIRECTION('center_axis',(0.,-1.,0.));
#11613=DIRECTION('ref_axis',(1.,0.,0.));
#11614=DIRECTION('',(-1.,0.,0.));
#11615=DIRECTION('',(0.,0.,1.));
#11616=DIRECTION('center_axis',(1.,0.,0.));
#11617=DIRECTION('ref_axis',(0.,0.,-1.));
#11618=DIRECTION('',(0.,1.,0.));
#11619=DIRECTION('',(0.,1.,0.));
#11620=DIRECTION('',(0.,0.,-1.));
#11621=DIRECTION('center_axis',(0.,0.,1.));
#11622=DIRECTION('ref_axis',(1.,0.,0.));
#11623=DIRECTION('',(1.,0.,0.));
#11624=DIRECTION('center_axis',(0.,1.,0.));
#11625=DIRECTION('ref_axis',(0.,0.,1.));
#11626=DIRECTION('center_axis',(0.,1.,0.));
#11627=DIRECTION('ref_axis',(1.,0.,0.));
#11628=DIRECTION('center_axis',(0.,1.,0.));
#11629=DIRECTION('ref_axis',(1.,0.,0.));
#11630=DIRECTION('center_axis',(0.,1.,0.));
#11631=DIRECTION('ref_axis',(1.,0.,0.));
#11632=DIRECTION('center_axis',(0.,1.,0.));
#11633=DIRECTION('ref_axis',(1.,0.,0.));
#11634=DIRECTION('center_axis',(0.,1.,0.));
#11635=DIRECTION('ref_axis',(1.,0.,0.));
#11636=DIRECTION('center_axis',(0.,1.,0.));
#11637=DIRECTION('ref_axis',(1.,0.,0.));
#11638=DIRECTION('center_axis',(0.,-1.,0.));
#11639=DIRECTION('ref_axis',(1.,0.,0.));
#11640=DIRECTION('center_axis',(0.,1.,0.));
#11641=DIRECTION('ref_axis',(1.,0.,0.));
#11642=DIRECTION('',(0.,-1.,0.));
#11643=DIRECTION('center_axis',(0.,1.,0.));
#11644=DIRECTION('ref_axis',(1.,0.,0.));
#11645=DIRECTION('',(0.,-1.,0.));
#11646=DIRECTION('center_axis',(0.,1.,0.));
#11647=DIRECTION('ref_axis',(1.,0.,0.));
#11648=DIRECTION('center_axis',(0.,1.,0.));
#11649=DIRECTION('ref_axis',(1.,0.,0.));
#11650=DIRECTION('center_axis',(0.,1.,0.));
#11651=DIRECTION('ref_axis',(1.,0.,0.));
#11652=DIRECTION('',(0.,-1.,0.));
#11653=DIRECTION('center_axis',(0.,1.,0.));
#11654=DIRECTION('ref_axis',(1.,0.,0.));
#11655=DIRECTION('center_axis',(0.,1.,0.));
#11656=DIRECTION('ref_axis',(1.,0.,0.));
#11657=DIRECTION('axis',(0.,0.,1.));
#11658=DIRECTION('refdir',(1.,0.,0.));
#11659=DIRECTION('center_axis',(0.,1.,0.));
#11660=DIRECTION('ref_axis',(1.,0.,0.));
#11661=DIRECTION('center_axis',(0.,-1.,0.));
#11662=DIRECTION('ref_axis',(1.,0.,0.));
#11663=DIRECTION('',(0.,-1.,0.));
#11664=DIRECTION('center_axis',(0.,-1.,0.));
#11665=DIRECTION('ref_axis',(1.,0.,0.));
#11666=DIRECTION('center_axis',(0.,1.,0.));
#11667=DIRECTION('ref_axis',(1.,0.,0.));
#11668=DIRECTION('center_axis',(0.,1.,0.));
#11669=DIRECTION('ref_axis',(1.,0.,0.));
#11670=DIRECTION('',(0.,-1.,0.));
#11671=DIRECTION('center_axis',(0.,1.,0.));
#11672=DIRECTION('ref_axis',(1.,0.,0.));
#11673=DIRECTION('center_axis',(0.,1.,0.));
#11674=DIRECTION('ref_axis',(1.,0.,0.));
#11675=DIRECTION('center_axis',(0.,1.,0.));
#11676=DIRECTION('ref_axis',(1.,0.,0.));
#11677=DIRECTION('axis',(0.,0.,1.));
#11678=DIRECTION('refdir',(1.,0.,0.));
#11679=DIRECTION('center_axis',(0.,0.,1.));
#11680=DIRECTION('ref_axis',(1.,0.,0.));
#11681=DIRECTION('',(0.,1.,0.));
#11682=DIRECTION('center_axis',(0.,0.,1.));
#11683=DIRECTION('ref_axis',(1.,0.,0.));
#11684=DIRECTION('center_axis',(0.,0.,1.));
#11685=DIRECTION('ref_axis',(1.,0.,0.));
#11686=DIRECTION('center_axis',(0.,0.,1.));
#11687=DIRECTION('ref_axis',(1.,0.,0.));
#11688=DIRECTION('',(0.,0.,1.));
#11689=DIRECTION('center_axis',(0.,0.,1.));
#11690=DIRECTION('ref_axis',(1.,0.,0.));
#11691=DIRECTION('center_axis',(0.,0.,1.));
#11692=DIRECTION('ref_axis',(1.,0.,0.));
#11693=DIRECTION('',(0.,-1.,0.));
#11694=DIRECTION('center_axis',(0.,1.,0.));
#11695=DIRECTION('ref_axis',(1.,0.,0.));
#11696=DIRECTION('center_axis',(0.,-1.,0.));
#11697=DIRECTION('ref_axis',(1.,0.,0.));
#11698=DIRECTION('',(0.,-1.,0.));
#11699=DIRECTION('center_axis',(0.,-1.,0.));
#11700=DIRECTION('ref_axis',(1.,0.,0.));
#11701=DIRECTION('center_axis',(0.,1.,0.));
#11702=DIRECTION('ref_axis',(1.,0.,0.));
#11703=DIRECTION('center_axis',(0.,1.,0.));
#11704=DIRECTION('ref_axis',(1.,0.,0.));
#11705=DIRECTION('',(0.,-1.,0.));
#11706=DIRECTION('center_axis',(0.,1.,0.));
#11707=DIRECTION('ref_axis',(1.,0.,0.));
#11708=DIRECTION('center_axis',(0.,1.,0.));
#11709=DIRECTION('ref_axis',(1.,0.,0.));
#11710=DIRECTION('center_axis',(0.,1.,0.));
#11711=DIRECTION('ref_axis',(1.,0.,0.));
#11712=DIRECTION('axis',(0.,0.,1.));
#11713=DIRECTION('refdir',(1.,0.,0.));
#11714=DIRECTION('center_axis',(-1.,0.,0.));
#11715=DIRECTION('ref_axis',(0.,0.,1.));
#11716=DIRECTION('',(0.,0.,1.));
#11717=DIRECTION('',(0.,1.,0.));
#11718=DIRECTION('',(0.,0.,-1.));
#11719=DIRECTION('',(0.,1.,0.));
#11720=DIRECTION('center_axis',(0.,0.,-1.));
#11721=DIRECTION('ref_axis',(-1.,0.,0.));
#11722=DIRECTION('',(-1.,0.,0.));
#11723=DIRECTION('',(0.,1.,0.));
#11724=DIRECTION('',(1.,0.,0.));
#11725=DIRECTION('center_axis',(1.,0.,0.));
#11726=DIRECTION('ref_axis',(0.,0.,-1.));
#11727=DIRECTION('',(0.,0.,-1.));
#11728=DIRECTION('',(0.,-1.,0.));
#11729=DIRECTION('',(0.,0.,1.));
#11730=DIRECTION('center_axis',(0.,1.,0.));
#11731=DIRECTION('ref_axis',(1.,0.,0.));
#11732=DIRECTION('center_axis',(0.,1.,0.));
#11733=DIRECTION('ref_axis',(1.,0.,0.));
#11734=DIRECTION('center_axis',(0.,-1.,0.));
#11735=DIRECTION('ref_axis',(1.,0.,0.));
#11736=DIRECTION('center_axis',(0.,1.,0.));
#11737=DIRECTION('ref_axis',(-1.83697019872103E-16,0.,1.));
#11738=DIRECTION('center_axis',(0.,-1.,0.));
#11739=DIRECTION('ref_axis',(1.,0.,0.));
#11740=DIRECTION('center_axis',(0.,1.,0.));
#11741=DIRECTION('ref_axis',(1.,0.,0.));
#11742=DIRECTION('center_axis',(0.,1.,0.));
#11743=DIRECTION('ref_axis',(1.,0.,0.));
#11744=DIRECTION('center_axis',(0.,-1.,0.));
#11745=DIRECTION('ref_axis',(1.,0.,0.));
#11746=DIRECTION('center_axis',(0.,1.,0.));
#11747=DIRECTION('ref_axis',(1.,0.,0.));
#11748=DIRECTION('',(0.,-1.,0.));
#11749=DIRECTION('center_axis',(0.,1.,0.));
#11750=DIRECTION('ref_axis',(1.,0.,0.));
#11751=DIRECTION('',(0.,-1.,0.));
#11752=DIRECTION('center_axis',(0.,1.,0.));
#11753=DIRECTION('ref_axis',(1.,0.,0.));
#11754=DIRECTION('center_axis',(0.,1.,0.));
#11755=DIRECTION('ref_axis',(1.,0.,0.));
#11756=DIRECTION('axis',(0.,0.,1.));
#11757=DIRECTION('refdir',(1.,0.,0.));
#11758=DIRECTION('center_axis',(0.,1.,0.));
#11759=DIRECTION('ref_axis',(1.,0.,0.));
#11760=DIRECTION('center_axis',(0.,-1.,0.));
#11761=DIRECTION('ref_axis',(1.,0.,0.));
#11762=DIRECTION('',(0.,-1.,0.));
#11763=DIRECTION('center_axis',(0.,-1.,0.));
#11764=DIRECTION('ref_axis',(1.,0.,0.));
#11765=DIRECTION('center_axis',(0.,1.,0.));
#11766=DIRECTION('ref_axis',(1.,0.,0.));
#11767=DIRECTION('center_axis',(0.,1.,0.));
#11768=DIRECTION('ref_axis',(1.,0.,0.));
#11769=DIRECTION('',(0.,-1.,0.));
#11770=DIRECTION('center_axis',(0.,1.,0.));
#11771=DIRECTION('ref_axis',(1.,0.,0.));
#11772=DIRECTION('center_axis',(0.,1.,0.));
#11773=DIRECTION('ref_axis',(1.,0.,0.));
#11774=DIRECTION('center_axis',(0.,1.,0.));
#11775=DIRECTION('ref_axis',(1.,0.,0.));
#11776=DIRECTION('axis',(0.,0.,1.));
#11777=DIRECTION('refdir',(1.,0.,0.));
#11778=DIRECTION('center_axis',(0.,1.,0.));
#11779=DIRECTION('ref_axis',(1.,0.,0.));
#11780=DIRECTION('center_axis',(0.,-1.,0.));
#11781=DIRECTION('ref_axis',(1.,0.,0.));
#11782=DIRECTION('',(0.,-1.,0.));
#11783=DIRECTION('center_axis',(0.,-1.,0.));
#11784=DIRECTION('ref_axis',(1.,0.,0.));
#11785=DIRECTION('center_axis',(0.,1.,0.));
#11786=DIRECTION('ref_axis',(1.,0.,0.));
#11787=DIRECTION('center_axis',(0.,1.,0.));
#11788=DIRECTION('ref_axis',(1.,0.,0.));
#11789=DIRECTION('',(0.,-1.,0.));
#11790=DIRECTION('center_axis',(0.,1.,0.));
#11791=DIRECTION('ref_axis',(1.,0.,0.));
#11792=DIRECTION('center_axis',(0.,1.,0.));
#11793=DIRECTION('ref_axis',(1.,0.,0.));
#11794=DIRECTION('center_axis',(0.,1.,0.));
#11795=DIRECTION('ref_axis',(1.,0.,0.));
#11796=DIRECTION('axis',(0.,0.,1.));
#11797=DIRECTION('refdir',(1.,0.,0.));
#11798=DIRECTION('center_axis',(0.,1.,0.));
#11799=DIRECTION('ref_axis',(0.,0.,1.));
#11800=DIRECTION('center_axis',(0.,-1.,0.));
#11801=DIRECTION('ref_axis',(1.,0.,0.));
#11802=DIRECTION('center_axis',(0.,-1.,0.));
#11803=DIRECTION('ref_axis',(1.,0.,0.));
#11804=DIRECTION('center_axis',(0.,-1.,0.));
#11805=DIRECTION('ref_axis',(1.,0.,0.));
#11806=DIRECTION('',(0.707106781186547,0.707106781186548,8.65956056235493E-17));
#11807=DIRECTION('center_axis',(0.,-1.,0.));
#11808=DIRECTION('ref_axis',(1.,0.,0.));
#11809=DIRECTION('center_axis',(0.,-1.,0.));
#11810=DIRECTION('ref_axis',(1.,0.,0.));
#11811=DIRECTION('',(0.,1.,0.));
#11812=DIRECTION('center_axis',(0.,1.,0.));
#11813=DIRECTION('ref_axis',(1.,0.,0.));
#11814=DIRECTION('center_axis',(0.,-1.,0.));
#11815=DIRECTION('ref_axis',(1.,0.,0.));
#11816=DIRECTION('',(-0.707106781186547,0.707106781186548,-8.65956056235493E-17));
#11817=DIRECTION('center_axis',(0.,-1.,0.));
#11818=DIRECTION('ref_axis',(0.,0.,-1.));
#11819=DIRECTION('center_axis',(0.,-1.,0.));
#11820=DIRECTION('ref_axis',(1.,0.,0.));
#11821=DIRECTION('center_axis',(0.,1.,0.));
#11822=DIRECTION('ref_axis',(1.,0.,0.));
#11823=DIRECTION('center_axis',(0.,1.,0.));
#11824=DIRECTION('ref_axis',(1.,0.,0.));
#11825=DIRECTION('',(-0.447213595499958,0.894427190999916,-5.47678698264203E-17));
#11826=DIRECTION('center_axis',(0.,-1.,0.));
#11827=DIRECTION('ref_axis',(1.,0.,0.));
#11828=DIRECTION('center_axis',(0.,1.,0.));
#11829=DIRECTION('ref_axis',(1.,0.,0.));
#11830=DIRECTION('',(0.,1.,0.));
#11831=DIRECTION('center_axis',(0.,1.,0.));
#11832=DIRECTION('ref_axis',(1.,0.,0.));
#11833=DIRECTION('center_axis',(0.,-1.,0.));
#11834=DIRECTION('ref_axis',(1.,0.,0.));
#11835=DIRECTION('',(-0.707106781186547,0.707106781186548,-8.65956056235493E-17));
#11836=DIRECTION('center_axis',(0.,-1.,0.));
#11837=DIRECTION('ref_axis',(0.,0.,-1.));
#11838=DIRECTION('center_axis',(0.866025403784439,0.,-0.5));
#11839=DIRECTION('ref_axis',(0.5,0.,0.866025403784439));
#11840=DIRECTION('',(-0.5,0.,-0.866025403784439));
#11841=DIRECTION('',(0.,-1.,0.));
#11842=DIRECTION('',(0.5,0.,0.866025403784439));
#11843=DIRECTION('',(0.,-1.,0.));
#11844=DIRECTION('center_axis',(1.60246890531964E-16,0.,-1.));
#11845=DIRECTION('ref_axis',(1.,0.,1.60246890531964E-16));
#11846=DIRECTION('',(-1.,0.,-1.60246890531964E-16));
#11847=DIRECTION('',(0.,-1.,0.));
#11848=DIRECTION('',(1.,0.,1.60246890531964E-16));
#11849=DIRECTION('center_axis',(-0.866025403784439,0.,-0.5));
#11850=DIRECTION('ref_axis',(0.5,0.,-0.866025403784439));
#11851=DIRECTION('',(-0.5,0.,0.866025403784439));
#11852=DIRECTION('',(0.,-1.,0.));
#11853=DIRECTION('',(0.5,0.,-0.866025403784439));
#11854=DIRECTION('center_axis',(-0.866025403784439,0.,0.5));
#11855=DIRECTION('ref_axis',(-0.5,0.,-0.866025403784439));
#11856=DIRECTION('',(0.5,0.,0.866025403784439));
#11857=DIRECTION('',(0.,-1.,0.));
#11858=DIRECTION('',(-0.5,0.,-0.866025403784439));
#11859=DIRECTION('center_axis',(-1.60246890531964E-16,0.,1.));
#11860=DIRECTION('ref_axis',(-1.,0.,-1.60246890531964E-16));
#11861=DIRECTION('',(1.,0.,1.60246890531964E-16));
#11862=DIRECTION('',(0.,-1.,0.));
#11863=DIRECTION('',(-1.,0.,-1.60246890531964E-16));
#11864=DIRECTION('center_axis',(0.866025403784439,0.,0.5));
#11865=DIRECTION('ref_axis',(-0.5,0.,0.866025403784439));
#11866=DIRECTION('',(0.5,0.,-0.866025403784439));
#11867=DIRECTION('',(-0.5,0.,0.866025403784439));
#11868=DIRECTION('center_axis',(0.,1.,0.));
#11869=DIRECTION('ref_axis',(1.,0.,0.));
#11870=DIRECTION('center_axis',(0.,-1.,0.));
#11871=DIRECTION('ref_axis',(0.,0.,-1.));
#11872=DIRECTION('',(0.,0.,1.));
#11873=DIRECTION('',(1.,0.,0.));
#11874=DIRECTION('',(0.,0.,1.));
#11875=DIRECTION('',(1.,0.,0.));
#11876=DIRECTION('',(0.,0.,1.));
#11877=DIRECTION('',(1.,0.,0.));
#11878=DIRECTION('',(0.,0.,1.));
#11879=DIRECTION('',(1.,0.,0.));
#11880=DIRECTION('',(0.,0.,1.));
#11881=DIRECTION('',(1.,0.,0.));
#11882=DIRECTION('',(0.,0.,1.));
#11883=DIRECTION('',(1.,0.,0.));
#11884=DIRECTION('',(0.,0.,1.));
#11885=DIRECTION('',(1.,0.,0.));
#11886=DIRECTION('',(0.,0.,1.));
#11887=DIRECTION('',(1.,0.,0.));
#11888=DIRECTION('',(0.,0.,1.));
#11889=DIRECTION('',(1.,0.,0.));
#11890=DIRECTION('',(0.,0.,1.));
#11891=DIRECTION('',(1.,0.,0.));
#11892=DIRECTION('',(0.,0.,1.));
#11893=DIRECTION('',(1.,0.,0.));
#11894=DIRECTION('',(0.,0.,1.));
#11895=DIRECTION('',(1.,0.,0.));
#11896=DIRECTION('',(0.,0.,1.));
#11897=DIRECTION('',(1.,0.,0.));
#11898=DIRECTION('',(0.,0.,1.));
#11899=DIRECTION('',(1.,0.,0.));
#11900=DIRECTION('',(0.,0.,1.));
#11901=DIRECTION('',(1.,0.,0.));
#11902=DIRECTION('',(0.,0.,1.));
#11903=DIRECTION('',(1.,0.,0.));
#11904=DIRECTION('',(0.,0.,1.));
#11905=DIRECTION('',(1.,0.,0.));
#11906=DIRECTION('',(0.,0.,1.));
#11907=DIRECTION('',(1.,0.,0.));
#11908=DIRECTION('',(0.,0.,1.));
#11909=DIRECTION('',(1.,0.,0.));
#11910=DIRECTION('',(0.,0.,1.));
#11911=DIRECTION('',(1.,0.,0.));
#11912=DIRECTION('',(0.,0.,1.));
#11913=DIRECTION('',(1.,0.,0.));
#11914=DIRECTION('',(0.,0.,1.));
#11915=DIRECTION('',(1.,0.,0.));
#11916=DIRECTION('',(0.,0.,1.));
#11917=DIRECTION('',(1.,0.,0.));
#11918=DIRECTION('',(0.,-1.,2.22044604925031E-16));
#11919=DIRECTION('',(1.,0.,0.));
#11920=DIRECTION('',(0.,-1.,2.22044604925031E-16));
#11921=DIRECTION('',(1.,0.,0.));
#11922=DIRECTION('',(0.,-1.,2.22044604925031E-16));
#11923=DIRECTION('',(1.,0.,0.));
#11924=DIRECTION('',(0.,-1.,2.22044604925031E-16));
#11925=DIRECTION('',(1.,0.,0.));
#11926=DIRECTION('',(0.,-1.,2.22044604925031E-16));
#11927=DIRECTION('',(1.,0.,0.));
#11928=DIRECTION('',(0.,-1.,2.22044604925031E-16));
#11929=DIRECTION('',(1.,0.,0.));
#11930=DIRECTION('',(0.,0.,1.));
#11931=DIRECTION('',(1.,0.,0.));
#11932=DIRECTION('',(0.,0.,1.));
#11933=DIRECTION('',(-1.,1.22464679914735E-16,0.));
#11934=DIRECTION('',(0.,0.,1.));
#11935=DIRECTION('',(-1.,1.22464679914735E-16,0.));
#11936=DIRECTION('',(0.,0.,1.));
#11937=DIRECTION('',(-1.,1.22464679914735E-16,0.));
#11938=DIRECTION('',(0.,0.,1.));
#11939=DIRECTION('',(-1.,1.22464679914735E-16,0.));
#11940=DIRECTION('',(0.,0.,1.));
#11941=DIRECTION('',(1.,0.,0.));
#11942=DIRECTION('',(0.,0.,1.));
#11943=DIRECTION('',(1.,0.,0.));
#11944=DIRECTION('',(0.,0.,1.));
#11945=DIRECTION('',(1.,0.,0.));
#11946=DIRECTION('',(0.,0.,1.));
#11947=DIRECTION('',(1.,0.,0.));
#11948=DIRECTION('',(0.,-1.,2.22044604925031E-16));
#11949=DIRECTION('',(1.,0.,0.));
#11950=DIRECTION('',(0.,-1.,2.22044604925031E-16));
#11951=DIRECTION('',(1.,0.,0.));
#11952=DIRECTION('',(0.,0.,1.));
#11953=DIRECTION('',(1.,0.,0.));
#11954=DIRECTION('',(0.,0.,1.));
#11955=DIRECTION('',(-1.,1.22464679914735E-16,0.));
#11956=DIRECTION('',(0.,0.,1.));
#11957=DIRECTION('',(-1.,1.22464679914735E-16,0.));
#11958=DIRECTION('',(0.,0.,1.));
#11959=DIRECTION('',(-1.,1.22464679914735E-16,0.));
#11960=DIRECTION('',(0.,0.,1.));
#11961=DIRECTION('',(-1.,1.22464679914735E-16,0.));
#11962=DIRECTION('',(0.,0.,1.));
#11963=DIRECTION('',(1.,0.,0.));
#11964=DIRECTION('',(0.,0.,1.));
#11965=DIRECTION('',(1.,0.,0.));
#11966=DIRECTION('',(0.,0.,1.));
#11967=DIRECTION('',(1.,0.,0.));
#11968=DIRECTION('',(0.,0.,1.));
#11969=DIRECTION('',(1.,0.,0.));
#11970=DIRECTION('',(0.,-1.,2.22044604925031E-16));
#11971=DIRECTION('',(1.,0.,0.));
#11972=DIRECTION('',(0.,-1.,2.22044604925031E-16));
#11973=DIRECTION('',(1.,0.,0.));
#11974=DIRECTION('',(0.,0.,1.));
#11975=DIRECTION('',(2.22044604925031E-16,-1.,0.));
#11976=DIRECTION('',(0.,0.,1.));
#11977=DIRECTION('',(2.22044604925031E-16,1.,0.));
#11978=DIRECTION('',(0.,0.,1.));
#11979=DIRECTION('',(2.22044604925031E-16,1.,0.));
#11980=DIRECTION('',(0.,0.,1.));
#11981=DIRECTION('',(2.22044604925031E-16,1.,0.));
#11982=DIRECTION('',(0.,0.,1.));
#11983=DIRECTION('',(2.22044604925031E-16,1.,0.));
#11984=DIRECTION('',(0.,0.,1.));
#11985=DIRECTION('',(2.22044604925031E-16,-1.,0.));
#11986=DIRECTION('',(0.,0.,1.));
#11987=DIRECTION('',(2.22044604925031E-16,-1.,0.));
#11988=DIRECTION('',(0.,0.,1.));
#11989=DIRECTION('',(2.22044604925031E-16,-1.,0.));
#11990=DIRECTION('',(0.,0.,1.));
#11991=DIRECTION('',(2.22044604925031E-16,-1.,0.));
#11992=DIRECTION('',(0.,-1.,2.22044604925031E-16));
#11993=DIRECTION('',(1.,0.,0.));
#11994=DIRECTION('',(0.,-1.,2.22044604925031E-16));
#11995=DIRECTION('',(1.,0.,0.));
#11996=DIRECTION('',(0.,0.,1.));
#11997=DIRECTION('',(2.22044604925031E-16,-1.,0.));
#11998=DIRECTION('',(0.,0.,1.));
#11999=DIRECTION('',(2.22044604925031E-16,1.,0.));
#12000=DIRECTION('',(0.,0.,1.));
#12001=DIRECTION('',(2.22044604925031E-16,1.,0.));
#12002=DIRECTION('',(0.,0.,1.));
#12003=DIRECTION('',(2.22044604925031E-16,1.,0.));
#12004=DIRECTION('',(0.,0.,1.));
#12005=DIRECTION('',(2.22044604925031E-16,1.,0.));
#12006=DIRECTION('',(0.,0.,1.));
#12007=DIRECTION('',(2.22044604925031E-16,-1.,0.));
#12008=DIRECTION('',(0.,0.,1.));
#12009=DIRECTION('',(2.22044604925031E-16,-1.,0.));
#12010=DIRECTION('',(0.,0.,1.));
#12011=DIRECTION('',(2.22044604925031E-16,-1.,0.));
#12012=DIRECTION('',(0.,0.,1.));
#12013=DIRECTION('',(2.22044604925031E-16,-1.,0.));
#12014=DIRECTION('',(0.,-1.,2.22044604925031E-16));
#12015=DIRECTION('',(1.,0.,0.));
#12016=DIRECTION('',(0.,-1.,2.22044604925031E-16));
#12017=DIRECTION('',(1.,0.,0.));
#12018=DIRECTION('',(0.,0.,1.));
#12019=DIRECTION('',(1.,0.,0.));
#12020=DIRECTION('',(0.,0.,1.));
#12021=DIRECTION('',(1.,0.,0.));
#12022=DIRECTION('',(0.,0.,1.));
#12023=DIRECTION('',(1.,0.,0.));
#12024=DIRECTION('',(0.,0.,1.));
#12025=DIRECTION('',(1.,0.,0.));
#12026=DIRECTION('axis',(0.,0.,1.));
#12027=DIRECTION('refdir',(1.,0.,0.));
#12028=DIRECTION('axis',(0.,0.,1.));
#12029=DIRECTION('refdir',(1.,0.,0.));
#12030=DIRECTION('center_axis',(0.,1.,0.));
#12031=DIRECTION('ref_axis',(0.,0.,1.));
#12032=DIRECTION('',(-1.,0.,0.));
#12033=DIRECTION('',(0.,0.,1.));
#12034=DIRECTION('',(1.,0.,0.));
#12035=DIRECTION('',(0.,0.,1.));
#12036=DIRECTION('center_axis',(1.,0.,0.));
#12037=DIRECTION('ref_axis',(0.,0.,-1.));
#12038=DIRECTION('center_axis',(-1.,0.,0.));
#12039=DIRECTION('ref_axis',(0.,0.,-1.));
#12040=DIRECTION('',(0.,-1.,0.));
#12041=DIRECTION('',(0.,0.,-1.));
#12042=DIRECTION('center_axis',(0.,0.,1.));
#12043=DIRECTION('ref_axis',(0.,-1.,0.));
#12044=DIRECTION('',(0.,-1.,0.));
#12045=DIRECTION('',(1.,0.,0.));
#12046=DIRECTION('center_axis',(0.,-1.,0.));
#12047=DIRECTION('ref_axis',(0.,0.,-1.));
#12048=DIRECTION('',(1.,0.,0.));
#12049=DIRECTION('',(0.,0.,-1.));
#12050=DIRECTION('center_axis',(1.,0.,0.));
#12051=DIRECTION('ref_axis',(0.,0.,-1.));
#12052=DIRECTION('center_axis',(1.,0.,0.));
#12053=DIRECTION('ref_axis',(0.,0.,-1.));
#12054=DIRECTION('center_axis',(1.,0.,0.));
#12055=DIRECTION('ref_axis',(0.,0.,-1.));
#12056=DIRECTION('center_axis',(1.,0.,0.));
#12057=DIRECTION('ref_axis',(0.,0.,-1.));
#12058=DIRECTION('center_axis',(1.,0.,0.));
#12059=DIRECTION('ref_axis',(0.,0.,-1.));
#12060=DIRECTION('center_axis',(1.,0.,0.));
#12061=DIRECTION('ref_axis',(0.,0.,-1.));
#12062=DIRECTION('center_axis',(1.,0.,0.));
#12063=DIRECTION('ref_axis',(0.,0.,-1.));
#12064=DIRECTION('center_axis',(-1.,0.,0.));
#12065=DIRECTION('ref_axis',(0.,0.,-1.));
#12066=DIRECTION('center_axis',(1.,0.,0.));
#12067=DIRECTION('ref_axis',(0.,0.,-1.));
#12068=DIRECTION('',(-1.,0.,0.));
#12069=DIRECTION('center_axis',(1.,0.,0.));
#12070=DIRECTION('ref_axis',(0.,0.,-1.));
#12071=DIRECTION('',(-1.,0.,0.));
#12072=DIRECTION('center_axis',(1.,0.,0.));
#12073=DIRECTION('ref_axis',(0.,0.,-1.));
#12074=DIRECTION('center_axis',(1.,0.,0.));
#12075=DIRECTION('ref_axis',(0.,0.,-1.));
#12076=DIRECTION('center_axis',(1.,0.,0.));
#12077=DIRECTION('ref_axis',(0.,0.,-1.));
#12078=DIRECTION('',(-1.,0.,0.));
#12079=DIRECTION('center_axis',(1.,0.,0.));
#12080=DIRECTION('ref_axis',(0.,0.,-1.));
#12081=DIRECTION('center_axis',(1.,0.,0.));
#12082=DIRECTION('ref_axis',(0.,0.,-1.));
#12083=DIRECTION('axis',(0.,0.,1.));
#12084=DIRECTION('refdir',(1.,0.,0.));
#12085=DIRECTION('center_axis',(0.,1.,0.));
#12086=DIRECTION('ref_axis',(0.,0.,1.));
#12087=DIRECTION('',(0.,0.,1.));
#12088=DIRECTION('',(1.,0.,0.));
#12089=DIRECTION('',(0.,0.,-1.));
#12090=DIRECTION('',(1.,0.,0.));
#12091=DIRECTION('center_axis',(0.,0.,-1.));
#12092=DIRECTION('ref_axis',(0.,1.,0.));
#12093=DIRECTION('',(0.,1.,0.));
#12094=DIRECTION('',(1.,0.,0.));
#12095=DIRECTION('',(0.,-1.,0.));
#12096=DIRECTION('center_axis',(0.,-1.,0.));
#12097=DIRECTION('ref_axis',(0.,0.,-1.));
#12098=DIRECTION('',(0.,0.,-1.));
#12099=DIRECTION('',(-1.,0.,0.));
#12100=DIRECTION('',(0.,0.,1.));
#12101=DIRECTION('center_axis',(1.,0.,0.));
#12102=DIRECTION('ref_axis',(0.,0.,-1.));
#12103=DIRECTION('center_axis',(1.,0.,0.));
#12104=DIRECTION('ref_axis',(0.,0.,-1.));
#12105=DIRECTION('center_axis',(-1.,0.,0.));
#12106=DIRECTION('ref_axis',(0.,0.,-1.));
#12107=DIRECTION('center_axis',(1.,0.,0.));
#12108=DIRECTION('ref_axis',(0.,1.22464679914735E-16,1.));
#12109=DIRECTION('center_axis',(-1.,0.,0.));
#12110=DIRECTION('ref_axis',(0.,0.,-1.));
#12111=DIRECTION('center_axis',(1.,0.,0.));
#12112=DIRECTION('ref_axis',(0.,0.,-1.));
#12113=DIRECTION('center_axis',(1.,0.,0.));
#12114=DIRECTION('ref_axis',(0.,0.,-1.));
#12115=DIRECTION('center_axis',(1.,0.,0.));
#12116=DIRECTION('ref_axis',(0.,0.,-1.));
#12117=DIRECTION('center_axis',(1.,0.,0.));
#12118=DIRECTION('ref_axis',(0.,0.,-1.));
#12119=DIRECTION('',(-1.,0.,0.));
#12120=DIRECTION('center_axis',(1.,0.,0.));
#12121=DIRECTION('ref_axis',(0.,0.,-1.));
#12122=DIRECTION('center_axis',(1.,0.,0.));
#12123=DIRECTION('ref_axis',(0.,0.,-1.));
#12124=DIRECTION('',(-1.,0.,0.));
#12125=DIRECTION('center_axis',(1.,0.,0.));
#12126=DIRECTION('ref_axis',(0.,0.,-1.));
#12127=DIRECTION('axis',(0.,0.,1.));
#12128=DIRECTION('refdir',(1.,0.,0.));
#12129=DIRECTION('center_axis',(1.,0.,0.));
#12130=DIRECTION('ref_axis',(0.,0.,-1.));
#12131=DIRECTION('center_axis',(-1.,0.,0.));
#12132=DIRECTION('ref_axis',(0.,0.,-1.));
#12133=DIRECTION('',(-1.,0.,0.));
#12134=DIRECTION('center_axis',(-1.,0.,0.));
#12135=DIRECTION('ref_axis',(0.,0.,-1.));
#12136=DIRECTION('center_axis',(1.,0.,0.));
#12137=DIRECTION('ref_axis',(0.,0.,-1.));
#12138=DIRECTION('center_axis',(1.,0.,0.));
#12139=DIRECTION('ref_axis',(0.,0.,-1.));
#12140=DIRECTION('',(-1.,0.,0.));
#12141=DIRECTION('center_axis',(1.,0.,0.));
#12142=DIRECTION('ref_axis',(0.,0.,-1.));
#12143=DIRECTION('center_axis',(1.,0.,0.));
#12144=DIRECTION('ref_axis',(0.,0.,-1.));
#12145=DIRECTION('center_axis',(1.,0.,0.));
#12146=DIRECTION('ref_axis',(0.,0.,-1.));
#12147=DIRECTION('axis',(0.,0.,1.));
#12148=DIRECTION('refdir',(1.,0.,0.));
#12149=DIRECTION('center_axis',(1.,0.,0.));
#12150=DIRECTION('ref_axis',(0.,0.,-1.));
#12151=DIRECTION('center_axis',(-1.,0.,0.));
#12152=DIRECTION('ref_axis',(0.,0.,-1.));
#12153=DIRECTION('',(-1.,0.,0.));
#12154=DIRECTION('center_axis',(-1.,0.,0.));
#12155=DIRECTION('ref_axis',(0.,0.,-1.));
#12156=DIRECTION('center_axis',(1.,0.,0.));
#12157=DIRECTION('ref_axis',(0.,0.,-1.));
#12158=DIRECTION('center_axis',(1.,0.,0.));
#12159=DIRECTION('ref_axis',(0.,0.,-1.));
#12160=DIRECTION('',(-1.,0.,0.));
#12161=DIRECTION('center_axis',(1.,0.,0.));
#12162=DIRECTION('ref_axis',(0.,0.,-1.));
#12163=DIRECTION('center_axis',(1.,0.,0.));
#12164=DIRECTION('ref_axis',(0.,0.,-1.));
#12165=DIRECTION('center_axis',(1.,0.,0.));
#12166=DIRECTION('ref_axis',(0.,0.,-1.));
#12167=DIRECTION('axis',(0.,0.,1.));
#12168=DIRECTION('refdir',(1.,0.,0.));
#12169=DIRECTION('center_axis',(0.,0.,1.));
#12170=DIRECTION('ref_axis',(1.,0.,0.));
#12171=DIRECTION('',(1.,0.,0.));
#12172=DIRECTION('center_axis',(0.,0.,1.));
#12173=DIRECTION('ref_axis',(1.,0.,0.));
#12174=DIRECTION('center_axis',(0.,0.,1.));
#12175=DIRECTION('ref_axis',(1.,0.,0.));
#12176=DIRECTION('center_axis',(0.,0.,1.));
#12177=DIRECTION('ref_axis',(1.,0.,0.));
#12178=DIRECTION('',(0.,0.,1.));
#12179=DIRECTION('center_axis',(0.,0.,1.));
#12180=DIRECTION('ref_axis',(1.,0.,0.));
#12181=DIRECTION('',(-1.,0.,0.));
#12182=DIRECTION('center_axis',(1.,0.,0.));
#12183=DIRECTION('ref_axis',(0.,0.,-1.));
#12184=DIRECTION('center_axis',(-1.,0.,0.));
#12185=DIRECTION('ref_axis',(0.,0.,-1.));
#12186=DIRECTION('',(-1.,0.,0.));
#12187=DIRECTION('',(-1.,0.,0.));
#12188=DIRECTION('center_axis',(-1.,0.,0.));
#12189=DIRECTION('ref_axis',(0.,0.,-1.));
#12190=DIRECTION('center_axis',(1.,0.,0.));
#12191=DIRECTION('ref_axis',(0.,0.,-1.));
#12192=DIRECTION('center_axis',(1.,0.,0.));
#12193=DIRECTION('ref_axis',(0.,0.,-1.));
#12194=DIRECTION('',(-1.,0.,0.));
#12195=DIRECTION('',(-1.,0.,0.));
#12196=DIRECTION('center_axis',(1.,0.,0.));
#12197=DIRECTION('ref_axis',(0.,0.,-1.));
#12198=DIRECTION('center_axis',(1.,0.,0.));
#12199=DIRECTION('ref_axis',(0.,0.,-1.));
#12200=DIRECTION('center_axis',(1.,0.,0.));
#12201=DIRECTION('ref_axis',(0.,0.,-1.));
#12202=DIRECTION('axis',(0.,0.,1.));
#12203=DIRECTION('refdir',(1.,0.,0.));
#12204=DIRECTION('center_axis',(0.,0.,1.));
#12205=DIRECTION('ref_axis',(1.,0.,0.));
#12206=DIRECTION('',(1.,0.,0.));
#12207=DIRECTION('center_axis',(0.,0.,1.));
#12208=DIRECTION('ref_axis',(1.,0.,0.));
#12209=DIRECTION('center_axis',(0.,0.,1.));
#12210=DIRECTION('ref_axis',(1.,0.,0.));
#12211=DIRECTION('center_axis',(0.,0.,1.));
#12212=DIRECTION('ref_axis',(1.,0.,0.));
#12213=DIRECTION('',(0.,0.,1.));
#12214=DIRECTION('center_axis',(0.,0.,1.));
#12215=DIRECTION('ref_axis',(1.,0.,0.));
#12216=DIRECTION('',(-1.,0.,0.));
#12217=DIRECTION('center_axis',(1.,0.,0.));
#12218=DIRECTION('ref_axis',(0.,0.,-1.));
#12219=DIRECTION('center_axis',(-1.,0.,0.));
#12220=DIRECTION('ref_axis',(0.,0.,-1.));
#12221=DIRECTION('',(-1.,0.,0.));
#12222=DIRECTION('',(-1.,0.,0.));
#12223=DIRECTION('center_axis',(-1.,0.,0.));
#12224=DIRECTION('ref_axis',(0.,0.,-1.));
#12225=DIRECTION('center_axis',(1.,0.,0.));
#12226=DIRECTION('ref_axis',(0.,0.,-1.));
#12227=DIRECTION('center_axis',(1.,0.,0.));
#12228=DIRECTION('ref_axis',(0.,0.,-1.));
#12229=DIRECTION('',(-1.,0.,0.));
#12230=DIRECTION('',(-1.,0.,0.));
#12231=DIRECTION('center_axis',(1.,0.,0.));
#12232=DIRECTION('ref_axis',(0.,0.,-1.));
#12233=DIRECTION('center_axis',(1.,0.,0.));
#12234=DIRECTION('ref_axis',(0.,0.,-1.));
#12235=DIRECTION('center_axis',(1.,0.,0.));
#12236=DIRECTION('ref_axis',(0.,0.,-1.));
#12237=DIRECTION('axis',(0.,0.,1.));
#12238=DIRECTION('refdir',(1.,0.,0.));
#12239=DIRECTION('center_axis',(1.,0.,0.));
#12240=DIRECTION('ref_axis',(0.,0.,-1.));
#12241=DIRECTION('',(0.,0.707106781186547,-0.707106781186548));
#12242=DIRECTION('',(0.,1.,0.));
#12243=DIRECTION('',(0.,0.707106781186547,0.707106781186548));
#12244=DIRECTION('',(0.,0.,1.));
#12245=DIRECTION('',(0.,-0.707106781186548,0.707106781186548));
#12246=DIRECTION('',(0.,-1.,0.));
#12247=DIRECTION('',(0.,-0.707106781186548,-0.707106781186548));
#12248=DIRECTION('',(0.,0.,-1.));
#12249=DIRECTION('center_axis',(0.,-0.707106781186548,-0.707106781186548));
#12250=DIRECTION('ref_axis',(-1.,0.,0.));
#12251=DIRECTION('',(-1.,0.,0.));
#12252=DIRECTION('',(0.,0.707106781186548,-0.707106781186548));
#12253=DIRECTION('',(1.,0.,0.));
#12254=DIRECTION('center_axis',(0.,-1.,0.));
#12255=DIRECTION('ref_axis',(1.,0.,0.));
#12256=DIRECTION('',(1.,0.,0.));
#12257=DIRECTION('',(0.,0.,-1.));
#12258=DIRECTION('center_axis',(0.,-0.707106781186548,0.707106781186547));
#12259=DIRECTION('ref_axis',(1.,0.,0.));
#12260=DIRECTION('',(-1.,0.,0.));
#12261=DIRECTION('',(0.,-0.707106781186547,-0.707106781186548));
#12262=DIRECTION('center_axis',(0.,0.,1.));
#12263=DIRECTION('ref_axis',(1.,0.,0.));
#12264=DIRECTION('',(1.,0.,0.));
#12265=DIRECTION('',(0.,-1.,0.));
#12266=DIRECTION('center_axis',(1.,0.,0.));
#12267=DIRECTION('ref_axis',(0.,0.,-1.));
#12268=DIRECTION('',(0.,-0.707106781186547,0.707106781186548));
#12269=DIRECTION('',(0.,0.,1.));
#12270=DIRECTION('',(0.,0.707106781186548,0.707106781186548));
#12271=DIRECTION('',(0.,1.,0.));
#12272=DIRECTION('center_axis',(0.,0.707106781186548,0.707106781186547));
#12273=DIRECTION('ref_axis',(1.,0.,0.));
#12274=DIRECTION('',(-1.,0.,0.));
#12275=DIRECTION('center_axis',(0.,1.,0.));
#12276=DIRECTION('ref_axis',(-1.,0.,0.));
#12277=DIRECTION('',(1.,0.,0.));
#12278=DIRECTION('center_axis',(0.,0.707106781186548,-0.707106781186548));
#12279=DIRECTION('ref_axis',(-1.,0.,0.));
#12280=DIRECTION('',(-1.,0.,0.));
#12281=DIRECTION('center_axis',(0.,0.,1.));
#12282=DIRECTION('ref_axis',(1.,0.,0.));
#12283=DIRECTION('axis',(0.,0.,1.));
#12284=DIRECTION('refdir',(1.,0.,0.));
#12285=DIRECTION('center_axis',(0.,1.,0.));
#12286=DIRECTION('ref_axis',(1.,0.,0.));
#12287=DIRECTION('center_axis',(0.,1.,0.));
#12288=DIRECTION('ref_axis',(1.,0.,0.));
#12289=DIRECTION('center_axis',(0.866025403784439,0.,-0.5));
#12290=DIRECTION('ref_axis',(0.5,0.,0.866025403784439));
#12291=DIRECTION('',(0.5,0.,0.866025403784439));
#12292=DIRECTION('',(0.,-1.,0.));
#12293=DIRECTION('',(0.5,0.,0.866025403784439));
#12294=DIRECTION('',(0.,-1.,0.));
#12295=DIRECTION('center_axis',(1.92296268638356E-16,0.,-1.));
#12296=DIRECTION('ref_axis',(1.,0.,1.92296268638356E-16));
#12297=DIRECTION('',(1.,0.,1.92296268638356E-16));
#12298=DIRECTION('',(0.,-1.,0.));
#12299=DIRECTION('',(1.,0.,1.92296268638356E-16));
#12300=DIRECTION('center_axis',(-0.866025403784439,0.,-0.5));
#12301=DIRECTION('ref_axis',(0.5,0.,-0.866025403784439));
#12302=DIRECTION('',(0.5,0.,-0.866025403784439));
#12303=DIRECTION('',(0.,-1.,0.));
#12304=DIRECTION('',(0.5,0.,-0.866025403784438));
#12305=DIRECTION('center_axis',(-0.866025403784439,0.,0.5));
#12306=DIRECTION('ref_axis',(-0.5,0.,-0.866025403784439));
#12307=DIRECTION('',(-0.5,0.,-0.866025403784439));
#12308=DIRECTION('',(0.,-1.,0.));
#12309=DIRECTION('',(-0.5,0.,-0.866025403784439));
#12310=DIRECTION('center_axis',(-1.92296268638356E-16,0.,1.));
#12311=DIRECTION('ref_axis',(-1.,0.,-1.92296268638356E-16));
#12312=DIRECTION('',(-1.,0.,-1.92296268638356E-16));
#12313=DIRECTION('',(0.,-1.,0.));
#12314=DIRECTION('',(-1.,0.,-1.92296268638356E-16));
#12315=DIRECTION('center_axis',(0.866025403784439,0.,0.5));
#12316=DIRECTION('ref_axis',(-0.5,0.,0.866025403784439));
#12317=DIRECTION('',(-0.5,0.,0.866025403784439));
#12318=DIRECTION('',(-0.5,0.,0.866025403784439));
#12319=DIRECTION('center_axis',(0.,-1.,0.));
#12320=DIRECTION('ref_axis',(0.,0.,-1.));
#12321=DIRECTION('center_axis',(0.,1.,0.));
#12322=DIRECTION('ref_axis',(0.,0.,1.));
#12323=DIRECTION('center_axis',(0.,-1.,0.));
#12324=DIRECTION('ref_axis',(1.,0.,0.));
#12325=DIRECTION('center_axis',(0.,-1.,0.));
#12326=DIRECTION('ref_axis',(1.,0.,0.));
#12327=DIRECTION('center_axis',(0.,-1.,0.));
#12328=DIRECTION('ref_axis',(1.,0.,0.));
#12329=DIRECTION('',(0.707106781186547,0.707106781186548,8.65956056235493E-17));
#12330=DIRECTION('center_axis',(0.,-1.,0.));
#12331=DIRECTION('ref_axis',(1.,0.,0.));
#12332=DIRECTION('',(0.,1.,0.));
#12333=DIRECTION('',(0.,0.,1.));
#12334=DIRECTION('',(1.,0.,0.));
#12335=DIRECTION('',(0.,0.,1.));
#12336=DIRECTION('',(1.,0.,0.));
#12337=DIRECTION('',(0.,0.,1.));
#12338=DIRECTION('',(1.,0.,0.));
#12339=DIRECTION('',(0.,0.,1.));
#12340=DIRECTION('',(1.,0.,0.));
#12341=DIRECTION('',(0.,0.,1.));
#12342=DIRECTION('',(1.,0.,0.));
#12343=DIRECTION('',(0.,0.,1.));
#12344=DIRECTION('',(1.,0.,0.));
#12345=DIRECTION('',(0.,-1.,2.22044604925031E-16));
#12346=DIRECTION('',(1.,0.,0.));
#12347=DIRECTION('',(8.65956056235493E-17,-8.65956056235493E-17,-1.));
#12348=DIRECTION('',(2.22044604925031E-16,1.,-8.65956056235494E-17));
#12349=DIRECTION('',(0.,0.,1.));
#12350=DIRECTION('',(1.,0.,0.));
#12351=DIRECTION('',(0.,0.,1.));
#12352=DIRECTION('',(1.,0.,0.));
#12353=DIRECTION('',(0.,0.,1.));
#12354=DIRECTION('',(1.,0.,0.));
#12355=DIRECTION('',(0.,0.,1.));
#12356=DIRECTION('',(1.,0.,0.));
#12357=DIRECTION('',(0.,0.,1.));
#12358=DIRECTION('',(1.,0.,0.));
#12359=DIRECTION('',(0.,0.,1.));
#12360=DIRECTION('',(1.,0.,0.));
#12361=DIRECTION('',(0.,0.,1.));
#12362=DIRECTION('',(1.,0.,0.));
#12363=DIRECTION('',(0.,-1.22464679914735E-16,-1.));
#12364=DIRECTION('',(1.,-7.49879891330929E-33,1.23259516440783E-32));
#12365=DIRECTION('',(0.,-1.,2.22044604925031E-16));
#12366=DIRECTION('',(1.,0.,0.));
#12367=DIRECTION('',(0.,-1.,2.22044604925031E-16));
#12368=DIRECTION('',(1.,0.,0.));
#12369=DIRECTION('',(0.,0.,1.));
#12370=DIRECTION('',(1.,0.,0.));
#12371=DIRECTION('',(0.,0.,1.));
#12372=DIRECTION('',(1.,0.,0.));
#12373=DIRECTION('',(0.,0.,1.));
#12374=DIRECTION('',(1.,0.,0.));
#12375=CARTESIAN_POINT('',(0.,0.,0.));
#12376=CARTESIAN_POINT('',(0.,0.,0.));
#12377=CARTESIAN_POINT('',(0.,0.,0.));
#12378=CARTESIAN_POINT('Origin',(7.,8.5,-0.1));
#12379=CARTESIAN_POINT('',(6.835,8.5,0.));
#12380=CARTESIAN_POINT('Origin',(7.,8.5,0.));
#12381=CARTESIAN_POINT('',(6.835,8.5,1.));
#12382=CARTESIAN_POINT('',(6.835,8.5,-0.1));
#12383=CARTESIAN_POINT('Origin',(7.,8.5,1.));
#12384=CARTESIAN_POINT('Origin',(-1.5,8.5,-0.1));
#12385=CARTESIAN_POINT('',(-1.665,8.5,0.));
#12386=CARTESIAN_POINT('Origin',(-1.5,8.5,0.));
#12387=CARTESIAN_POINT('',(-1.665,8.5,1.));
#12388=CARTESIAN_POINT('',(-1.665,8.5,-0.1));
#12389=CARTESIAN_POINT('Origin',(-1.5,8.5,1.));
#12390=CARTESIAN_POINT('Origin',(-2.9,-4.,-0.1));
#12391=CARTESIAN_POINT('',(-3.065,-4.,0.));
#12392=CARTESIAN_POINT('Origin',(-2.9,-4.,0.));
#12393=CARTESIAN_POINT('',(-3.065,-4.,1.));
#12394=CARTESIAN_POINT('',(-3.065,-4.,-0.1));
#12395=CARTESIAN_POINT('Origin',(-2.9,-4.,1.));
#12396=CARTESIAN_POINT('Origin',(2.9,-4.,-0.1));
#12397=CARTESIAN_POINT('',(2.735,-4.,0.));
#12398=CARTESIAN_POINT('Origin',(2.9,-4.,0.));
#12399=CARTESIAN_POINT('',(2.735,-4.,1.));
#12400=CARTESIAN_POINT('',(2.735,-4.,-0.1));
#12401=CARTESIAN_POINT('Origin',(2.9,-4.,1.));
#12402=CARTESIAN_POINT('Origin',(-2.9,-7.,-0.1));
#12403=CARTESIAN_POINT('',(-3.065,-7.,0.));
#12404=CARTESIAN_POINT('Origin',(-2.9,-7.,0.));
#12405=CARTESIAN_POINT('',(-3.065,-7.,1.));
#12406=CARTESIAN_POINT('',(-3.065,-7.,-0.1));
#12407=CARTESIAN_POINT('Origin',(-2.9,-7.,1.));
#12408=CARTESIAN_POINT('Origin',(2.9,-7.,-0.1));
#12409=CARTESIAN_POINT('',(2.735,-7.,0.));
#12410=CARTESIAN_POINT('Origin',(2.9,-7.,0.));
#12411=CARTESIAN_POINT('',(2.735,-7.,1.));
#12412=CARTESIAN_POINT('',(2.735,-7.,-0.1));
#12413=CARTESIAN_POINT('Origin',(2.9,-7.,1.));
#12414=CARTESIAN_POINT('Origin',(8.3,1.2,-0.1));
#12415=CARTESIAN_POINT('',(8.09,1.2,0.));
#12416=CARTESIAN_POINT('Origin',(8.3,1.2,0.));
#12417=CARTESIAN_POINT('',(8.09,1.2,1.));
#12418=CARTESIAN_POINT('',(8.09,1.2,-0.1));
#12419=CARTESIAN_POINT('Origin',(8.3,1.2,1.));
#12420=CARTESIAN_POINT('Origin',(-2.8,5.3,-0.1));
#12421=CARTESIAN_POINT('',(-3.01,5.3,0.));
#12422=CARTESIAN_POINT('Origin',(-2.8,5.3,0.));
#12423=CARTESIAN_POINT('',(-3.01,5.3,1.));
#12424=CARTESIAN_POINT('',(-3.01,5.3,-0.1));
#12425=CARTESIAN_POINT('Origin',(-2.8,5.3,1.));
#12426=CARTESIAN_POINT('Origin',(-2.8,1.2,-0.1));
#12427=CARTESIAN_POINT('',(-3.01,1.2,0.));
#12428=CARTESIAN_POINT('Origin',(-2.8,1.2,0.));
#12429=CARTESIAN_POINT('',(-3.01,1.2,1.));
#12430=CARTESIAN_POINT('',(-3.01,1.2,-0.1));
#12431=CARTESIAN_POINT('Origin',(-2.8,1.2,1.));
#12432=CARTESIAN_POINT('Origin',(8.3,5.3,-0.1));
#12433=CARTESIAN_POINT('',(8.09,5.3,0.));
#12434=CARTESIAN_POINT('Origin',(8.3,5.3,0.));
#12435=CARTESIAN_POINT('',(8.09,5.3,1.));
#12436=CARTESIAN_POINT('',(8.09,5.3,-0.1));
#12437=CARTESIAN_POINT('Origin',(8.3,5.3,1.));
#12438=CARTESIAN_POINT('Origin',(10.,11.,0.));
#12439=CARTESIAN_POINT('',(10.,11.,0.));
#12440=CARTESIAN_POINT('',(-6.,11.,0.));
#12441=CARTESIAN_POINT('',(10.,11.,0.));
#12442=CARTESIAN_POINT('',(-6.,11.,1.));
#12443=CARTESIAN_POINT('',(-6.,11.,0.));
#12444=CARTESIAN_POINT('',(10.,11.,1.));
#12445=CARTESIAN_POINT('',(10.,11.,1.));
#12446=CARTESIAN_POINT('',(10.,11.,0.));
#12447=CARTESIAN_POINT('Origin',(10.,-11.,0.));
#12448=CARTESIAN_POINT('',(10.,-11.,0.));
#12449=CARTESIAN_POINT('',(10.,-11.,0.));
#12450=CARTESIAN_POINT('',(10.,-11.,1.));
#12451=CARTESIAN_POINT('',(10.,-11.,1.));
#12452=CARTESIAN_POINT('',(10.,-11.,0.));
#12453=CARTESIAN_POINT('Origin',(-6.,-11.,0.));
#12454=CARTESIAN_POINT('',(-6.,-11.,0.));
#12455=CARTESIAN_POINT('',(-6.,-11.,0.));
#12456=CARTESIAN_POINT('',(-6.,-11.,1.));
#12457=CARTESIAN_POINT('',(-6.,-11.,1.));
#12458=CARTESIAN_POINT('',(-6.,-11.,0.));
#12459=CARTESIAN_POINT('Origin',(-6.,11.,0.));
#12460=CARTESIAN_POINT('',(-6.,11.,0.));
#12461=CARTESIAN_POINT('',(-6.,11.,1.));
#12462=CARTESIAN_POINT('Origin',(2.,0.,1.));
#12463=CARTESIAN_POINT('Origin',(2.,0.,0.));
#12464=CARTESIAN_POINT('',(0.,0.,0.));
#12465=CARTESIAN_POINT('Origin',(10.,-9.,-0.4));
#12466=CARTESIAN_POINT('',(10.,-9.,-0.4));
#12467=CARTESIAN_POINT('',(-6.,-9.,-0.4));
#12468=CARTESIAN_POINT('',(10.,-9.,-0.4));
#12469=CARTESIAN_POINT('',(-6.,-9.,0.));
#12470=CARTESIAN_POINT('',(-6.,-9.,-0.4));
#12471=CARTESIAN_POINT('',(10.,-9.,0.));
#12472=CARTESIAN_POINT('',(10.,-9.,0.));
#12473=CARTESIAN_POINT('',(10.,-9.,-0.4));
#12474=CARTESIAN_POINT('Origin',(10.,-10.,-0.4));
#12475=CARTESIAN_POINT('',(10.,-10.,-0.4));
#12476=CARTESIAN_POINT('',(10.,-10.,-0.4));
#12477=CARTESIAN_POINT('',(10.,-10.,0.));
#12478=CARTESIAN_POINT('',(10.,-10.,0.));
#12479=CARTESIAN_POINT('',(10.,-10.,-0.4));
#12480=CARTESIAN_POINT('Origin',(-6.,-10.,-0.4));
#12481=CARTESIAN_POINT('',(-6.,-10.,-0.4));
#12482=CARTESIAN_POINT('',(-6.,-10.,-0.4));
#12483=CARTESIAN_POINT('',(-6.,-10.,0.));
#12484=CARTESIAN_POINT('',(-6.,-10.,0.));
#12485=CARTESIAN_POINT('',(-6.,-10.,-0.4));
#12486=CARTESIAN_POINT('Origin',(-6.,-9.,-0.4));
#12487=CARTESIAN_POINT('',(-6.,-9.,-0.4));
#12488=CARTESIAN_POINT('',(-6.,-9.,0.));
#12489=CARTESIAN_POINT('Origin',(2.,-9.5,0.));
#12490=CARTESIAN_POINT('Origin',(2.,-9.5,-0.4));
#12491=CARTESIAN_POINT('',(0.,0.,0.));
#12492=CARTESIAN_POINT('Origin',(10.,10.5,-0.4));
#12493=CARTESIAN_POINT('',(10.,10.5,-0.4));
#12494=CARTESIAN_POINT('',(-6.,10.5,-0.4));
#12495=CARTESIAN_POINT('',(10.,10.5,-0.4));
#12496=CARTESIAN_POINT('',(-6.,10.5,0.));
#12497=CARTESIAN_POINT('',(-6.,10.5,-0.4));
#12498=CARTESIAN_POINT('',(10.,10.5,0.));
#12499=CARTESIAN_POINT('',(10.,10.5,0.));
#12500=CARTESIAN_POINT('',(10.,10.5,-0.4));
#12501=CARTESIAN_POINT('Origin',(10.,9.5,-0.4));
#12502=CARTESIAN_POINT('',(10.,9.5,-0.4));
#12503=CARTESIAN_POINT('',(10.,9.5,-0.4));
#12504=CARTESIAN_POINT('',(10.,9.5,0.));
#12505=CARTESIAN_POINT('',(10.,9.5,0.));
#12506=CARTESIAN_POINT('',(10.,9.5,-0.4));
#12507=CARTESIAN_POINT('Origin',(-6.,9.5,-0.4));
#12508=CARTESIAN_POINT('',(-6.,9.5,-0.4));
#12509=CARTESIAN_POINT('',(-6.,9.5,-0.4));
#12510=CARTESIAN_POINT('',(-6.,9.5,0.));
#12511=CARTESIAN_POINT('',(-6.,9.5,0.));
#12512=CARTESIAN_POINT('',(-6.,9.5,-0.4));
#12513=CARTESIAN_POINT('Origin',(-6.,10.5,-0.4));
#12514=CARTESIAN_POINT('',(-6.,10.5,-0.4));
#12515=CARTESIAN_POINT('',(-6.,10.5,0.));
#12516=CARTESIAN_POINT('Origin',(2.,10.,0.));
#12517=CARTESIAN_POINT('Origin',(2.,10.,-0.4));
#12518=CARTESIAN_POINT('',(0.,0.,0.));
#12519=CARTESIAN_POINT('Origin',(4.1,1.5,0.9));
#12520=CARTESIAN_POINT('',(3.935,1.5,1.));
#12521=CARTESIAN_POINT('Origin',(4.1,1.5,1.));
#12522=CARTESIAN_POINT('',(3.935,1.5,2.));
#12523=CARTESIAN_POINT('',(3.935,1.5,0.9));
#12524=CARTESIAN_POINT('Origin',(4.1,1.5,2.));
#12525=CARTESIAN_POINT('Origin',(6.9,4.5,0.9));
#12526=CARTESIAN_POINT('',(6.735,4.5,1.));
#12527=CARTESIAN_POINT('Origin',(6.9,4.5,1.));
#12528=CARTESIAN_POINT('',(6.735,4.5,2.));
#12529=CARTESIAN_POINT('',(6.735,4.5,0.9));
#12530=CARTESIAN_POINT('Origin',(6.9,4.5,2.));
#12531=CARTESIAN_POINT('Origin',(-1.7,1.5,0.9));
#12532=CARTESIAN_POINT('',(-1.865,1.5,1.));
#12533=CARTESIAN_POINT('Origin',(-1.7,1.5,1.));
#12534=CARTESIAN_POINT('',(-1.865,1.5,2.));
#12535=CARTESIAN_POINT('',(-1.865,1.5,0.9));
#12536=CARTESIAN_POINT('Origin',(-1.7,1.5,2.));
#12537=CARTESIAN_POINT('Origin',(1.1,4.5,0.9));
#12538=CARTESIAN_POINT('',(0.935,4.5,1.));
#12539=CARTESIAN_POINT('Origin',(1.1,4.5,1.));
#12540=CARTESIAN_POINT('',(0.935,4.5,2.));
#12541=CARTESIAN_POINT('',(0.935,4.5,0.9));
#12542=CARTESIAN_POINT('Origin',(1.1,4.5,2.));
#12543=CARTESIAN_POINT('Origin',(8.3,5.1,0.9));
#12544=CARTESIAN_POINT('',(8.025,5.1,1.));
#12545=CARTESIAN_POINT('',(8.025,5.1,2.));
#12546=CARTESIAN_POINT('',(8.025,5.1,0.9));
#12547=CARTESIAN_POINT('',(8.575,5.1,2.));
#12548=CARTESIAN_POINT('Origin',(8.3,5.1,2.));
#12549=CARTESIAN_POINT('',(8.575,5.1,1.));
#12550=CARTESIAN_POINT('',(8.575,5.1,0.9));
#12551=CARTESIAN_POINT('Origin',(8.3,5.1,1.));
#12552=CARTESIAN_POINT('Origin',(8.3,5.5,0.9));
#12553=CARTESIAN_POINT('',(8.575,5.5,1.));
#12554=CARTESIAN_POINT('',(8.575,5.5,2.));
#12555=CARTESIAN_POINT('',(8.575,5.5,0.9));
#12556=CARTESIAN_POINT('',(8.025,5.5,2.));
#12557=CARTESIAN_POINT('Origin',(8.3,5.5,2.));
#12558=CARTESIAN_POINT('',(8.025,5.5,1.));
#12559=CARTESIAN_POINT('',(8.025,5.5,0.9));
#12560=CARTESIAN_POINT('Origin',(8.3,5.5,1.));
#12561=CARTESIAN_POINT('Origin',(2.75,3.25,2.));
#12562=CARTESIAN_POINT('',(-3.5,6.,2.));
#12563=CARTESIAN_POINT('',(-3.5,0.5,2.));
#12564=CARTESIAN_POINT('',(-3.5,6.,2.));
#12565=CARTESIAN_POINT('',(9.,0.5,2.));
#12566=CARTESIAN_POINT('',(-3.5,0.5,2.));
#12567=CARTESIAN_POINT('',(9.,6.,2.));
#12568=CARTESIAN_POINT('',(9.,0.5,2.));
#12569=CARTESIAN_POINT('',(9.,6.,2.));
#12570=CARTESIAN_POINT('',(8.025,4.375,2.));
#12571=CARTESIAN_POINT('',(8.575,4.175,2.));
#12572=CARTESIAN_POINT('',(-2.525,5.1,2.));
#12573=CARTESIAN_POINT('',(-3.075,5.1,2.));
#12574=CARTESIAN_POINT('Origin',(-2.8,5.1,2.));
#12575=CARTESIAN_POINT('',(-3.075,5.5,2.));
#12576=CARTESIAN_POINT('',(-3.075,4.375,2.));
#12577=CARTESIAN_POINT('',(-2.525,5.5,2.));
#12578=CARTESIAN_POINT('Origin',(-2.8,5.5,2.));
#12579=CARTESIAN_POINT('',(-2.525,4.175,2.));
#12580=CARTESIAN_POINT('',(-2.525,1.,2.));
#12581=CARTESIAN_POINT('',(-3.075,1.,2.));
#12582=CARTESIAN_POINT('Origin',(-2.8,1.,2.));
#12583=CARTESIAN_POINT('',(-3.075,1.4,2.));
#12584=CARTESIAN_POINT('',(-3.075,2.325,2.));
#12585=CARTESIAN_POINT('',(-2.525,1.4,2.));
#12586=CARTESIAN_POINT('Origin',(-2.8,1.4,2.));
#12587=CARTESIAN_POINT('',(-2.525,2.125,2.));
#12588=CARTESIAN_POINT('',(8.575,1.,2.));
#12589=CARTESIAN_POINT('',(8.025,1.,2.));
#12590=CARTESIAN_POINT('Origin',(8.3,1.,2.));
#12591=CARTESIAN_POINT('',(8.025,1.4,2.));
#12592=CARTESIAN_POINT('',(8.025,2.325,2.));
#12593=CARTESIAN_POINT('',(8.575,1.4,2.));
#12594=CARTESIAN_POINT('Origin',(8.3,1.4,2.));
#12595=CARTESIAN_POINT('',(8.575,2.125,2.));
#12596=CARTESIAN_POINT('Origin',(8.025,5.5,0.9));
#12597=CARTESIAN_POINT('',(8.025,4.375,1.));
#12598=CARTESIAN_POINT('Origin',(8.575,5.1,0.9));
#12599=CARTESIAN_POINT('',(8.575,4.175,1.));
#12600=CARTESIAN_POINT('Origin',(8.3,1.,0.9));
#12601=CARTESIAN_POINT('',(8.025,1.,1.));
#12602=CARTESIAN_POINT('',(8.025,1.,0.9));
#12603=CARTESIAN_POINT('',(8.575,1.,1.));
#12604=CARTESIAN_POINT('',(8.575,1.,0.9));
#12605=CARTESIAN_POINT('Origin',(8.3,1.,1.));
#12606=CARTESIAN_POINT('Origin',(8.3,1.4,0.9));
#12607=CARTESIAN_POINT('',(8.575,1.4,1.));
#12608=CARTESIAN_POINT('',(8.575,1.4,0.9));
#12609=CARTESIAN_POINT('',(8.025,1.4,1.));
#12610=CARTESIAN_POINT('',(8.025,1.4,0.9));
#12611=CARTESIAN_POINT('Origin',(8.3,1.4,1.));
#12612=CARTESIAN_POINT('Origin',(8.025,1.4,0.9));
#12613=CARTESIAN_POINT('',(8.025,2.325,1.));
#12614=CARTESIAN_POINT('Origin',(8.575,1.,0.9));
#12615=CARTESIAN_POINT('',(8.575,2.125,1.));
#12616=CARTESIAN_POINT('Origin',(-2.8,5.1,0.9));
#12617=CARTESIAN_POINT('',(-3.075,5.1,1.));
#12618=CARTESIAN_POINT('',(-3.075,5.1,0.9));
#12619=CARTESIAN_POINT('',(-2.525,5.1,1.));
#12620=CARTESIAN_POINT('',(-2.525,5.1,0.9));
#12621=CARTESIAN_POINT('Origin',(-2.8,5.1,1.));
#12622=CARTESIAN_POINT('Origin',(-2.8,5.5,0.9));
#12623=CARTESIAN_POINT('',(-2.525,5.5,1.));
#12624=CARTESIAN_POINT('',(-2.525,5.5,0.9));
#12625=CARTESIAN_POINT('',(-3.075,5.5,1.));
#12626=CARTESIAN_POINT('',(-3.075,5.5,0.9));
#12627=CARTESIAN_POINT('Origin',(-2.8,5.5,1.));
#12628=CARTESIAN_POINT('Origin',(-3.075,5.5,0.9));
#12629=CARTESIAN_POINT('',(-3.075,4.375,1.));
#12630=CARTESIAN_POINT('Origin',(-2.525,5.1,0.9));
#12631=CARTESIAN_POINT('',(-2.525,4.175,1.));
#12632=CARTESIAN_POINT('Origin',(-2.8,1.,0.9));
#12633=CARTESIAN_POINT('',(-3.075,1.,1.));
#12634=CARTESIAN_POINT('',(-3.075,1.,0.9));
#12635=CARTESIAN_POINT('',(-2.525,1.,1.));
#12636=CARTESIAN_POINT('',(-2.525,1.,0.9));
#12637=CARTESIAN_POINT('Origin',(-2.8,1.,1.));
#12638=CARTESIAN_POINT('Origin',(-2.8,1.4,0.9));
#12639=CARTESIAN_POINT('',(-2.525,1.4,1.));
#12640=CARTESIAN_POINT('',(-2.525,1.4,0.9));
#12641=CARTESIAN_POINT('',(-3.075,1.4,1.));
#12642=CARTESIAN_POINT('',(-3.075,1.4,0.9));
#12643=CARTESIAN_POINT('Origin',(-2.8,1.4,1.));
#12644=CARTESIAN_POINT('Origin',(-3.075,1.4,0.9));
#12645=CARTESIAN_POINT('',(-3.075,2.325,1.));
#12646=CARTESIAN_POINT('Origin',(-2.525,1.,0.9));
#12647=CARTESIAN_POINT('',(-2.525,2.125,1.));
#12648=CARTESIAN_POINT('Origin',(9.,6.,1.));
#12649=CARTESIAN_POINT('',(9.,6.,1.));
#12650=CARTESIAN_POINT('',(-3.5,6.,1.));
#12651=CARTESIAN_POINT('',(9.,6.,1.));
#12652=CARTESIAN_POINT('',(-3.5,6.,1.));
#12653=CARTESIAN_POINT('',(9.,6.,1.));
#12654=CARTESIAN_POINT('Origin',(9.,0.5,1.));
#12655=CARTESIAN_POINT('',(9.,0.5,1.));
#12656=CARTESIAN_POINT('',(9.,0.5,1.));
#12657=CARTESIAN_POINT('',(9.,0.5,1.));
#12658=CARTESIAN_POINT('Origin',(-3.5,0.5,1.));
#12659=CARTESIAN_POINT('',(-3.5,0.5,1.));
#12660=CARTESIAN_POINT('',(-3.5,0.5,1.));
#12661=CARTESIAN_POINT('',(-3.5,0.5,1.));
#12662=CARTESIAN_POINT('Origin',(-3.5,6.,1.));
#12663=CARTESIAN_POINT('',(-3.5,6.,1.));
#12664=CARTESIAN_POINT('Origin',(2.75,3.25,1.));
#12665=CARTESIAN_POINT('',(0.,0.,0.));
#12666=CARTESIAN_POINT('Origin',(-1.48492424049175,-7.9,5.51507575950825));
#12667=CARTESIAN_POINT('',(-1.64992424049175,-7.8,5.51507575950825));
#12668=CARTESIAN_POINT('Origin',(-1.48492424049175,-7.8,5.51507575950825));
#12669=CARTESIAN_POINT('',(-1.64992424049175,-6.2,5.51507575950825));
#12670=CARTESIAN_POINT('',(-1.64992424049175,-7.9,5.51507575950825));
#12671=CARTESIAN_POINT('Origin',(-1.48492424049175,-6.2,5.51507575950825));
#12672=CARTESIAN_POINT('Origin',(-1.48492424049175,-7.9,8.48492424049175));
#12673=CARTESIAN_POINT('',(-1.64992424049175,-7.8,8.48492424049175));
#12674=CARTESIAN_POINT('Origin',(-1.48492424049175,-7.8,8.48492424049175));
#12675=CARTESIAN_POINT('',(-1.64992424049175,-6.2,8.48492424049175));
#12676=CARTESIAN_POINT('',(-1.64992424049175,-7.9,8.48492424049175));
#12677=CARTESIAN_POINT('Origin',(-1.48492424049175,-6.2,8.48492424049175));
#12678=CARTESIAN_POINT('Origin',(1.48492424049175,-7.9,8.48492424049175));
#12679=CARTESIAN_POINT('',(1.31992424049175,-7.8,8.48492424049175));
#12680=CARTESIAN_POINT('Origin',(1.48492424049175,-7.8,8.48492424049175));
#12681=CARTESIAN_POINT('',(1.31992424049175,-6.2,8.48492424049175));
#12682=CARTESIAN_POINT('',(1.31992424049175,-7.9,8.48492424049175));
#12683=CARTESIAN_POINT('Origin',(1.48492424049175,-6.2,8.48492424049175));
#12684=CARTESIAN_POINT('Origin',(1.48492424049175,-7.9,5.51507575950825));
#12685=CARTESIAN_POINT('',(1.31992424049175,-7.8,5.51507575950825));
#12686=CARTESIAN_POINT('Origin',(1.48492424049175,-7.8,5.51507575950825));
#12687=CARTESIAN_POINT('',(1.31992424049175,-6.2,5.51507575950825));
#12688=CARTESIAN_POINT('',(1.31992424049175,-7.9,5.51507575950825));
#12689=CARTESIAN_POINT('Origin',(1.48492424049175,-6.2,5.51507575950825));
#12690=CARTESIAN_POINT('Origin',(0.,-7.9,7.));
#12691=CARTESIAN_POINT('',(-1.6,-7.8,7.));
#12692=CARTESIAN_POINT('Origin',(0.,-7.8,7.));
#12693=CARTESIAN_POINT('',(-1.6,-6.2,7.));
#12694=CARTESIAN_POINT('',(-1.6,-7.9,7.));
#12695=CARTESIAN_POINT('Origin',(0.,-6.2,7.));
#12696=CARTESIAN_POINT('Origin',(-2.9,-7.,0.9));
#12697=CARTESIAN_POINT('',(-3.125,-7.,1.));
#12698=CARTESIAN_POINT('Origin',(-2.9,-7.,1.));
#12699=CARTESIAN_POINT('',(-3.125,-7.,1.8));
#12700=CARTESIAN_POINT('',(-3.125,-7.,0.9));
#12701=CARTESIAN_POINT('Origin',(-2.9,-7.,1.8));
#12702=CARTESIAN_POINT('Origin',(2.9,-7.,0.9));
#12703=CARTESIAN_POINT('',(2.675,-7.,1.));
#12704=CARTESIAN_POINT('Origin',(2.9,-7.,1.));
#12705=CARTESIAN_POINT('',(2.675,-7.,1.8));
#12706=CARTESIAN_POINT('',(2.675,-7.,0.9));
#12707=CARTESIAN_POINT('Origin',(2.9,-7.,1.8));
#12708=CARTESIAN_POINT('Origin',(-3.5,-7.8,1.8));
#12709=CARTESIAN_POINT('',(2.4,-7.8,1.8));
#12710=CARTESIAN_POINT('',(2.4,-6.2,1.8));
#12711=CARTESIAN_POINT('',(2.4,-7.8,1.8));
#12712=CARTESIAN_POINT('',(3.5,-7.8,1.8));
#12713=CARTESIAN_POINT('',(3.5,-7.8,1.8));
#12714=CARTESIAN_POINT('',(3.5,-6.2,1.8));
#12715=CARTESIAN_POINT('',(3.5,-7.8,1.8));
#12716=CARTESIAN_POINT('',(3.5,-6.2,1.8));
#12717=CARTESIAN_POINT('Origin',(-3.5,-7.8,1.8));
#12718=CARTESIAN_POINT('',(-2.4,-6.2,1.8));
#12719=CARTESIAN_POINT('',(-2.4,-7.8,1.8));
#12720=CARTESIAN_POINT('',(-2.4,-7.,1.8));
#12721=CARTESIAN_POINT('',(-3.5,-6.2,1.8));
#12722=CARTESIAN_POINT('',(3.5,-6.2,1.8));
#12723=CARTESIAN_POINT('',(-3.5,-7.8,1.8));
#12724=CARTESIAN_POINT('',(-3.5,-7.8,1.8));
#12725=CARTESIAN_POINT('',(3.5,-7.8,1.8));
#12726=CARTESIAN_POINT('Origin',(-3.5,-7.8,1.));
#12727=CARTESIAN_POINT('',(-3.5,-7.8,1.));
#12728=CARTESIAN_POINT('',(-3.5,-7.8,1.8));
#12729=CARTESIAN_POINT('',(-3.5,-6.2,1.));
#12730=CARTESIAN_POINT('',(-3.5,-6.2,1.8));
#12731=CARTESIAN_POINT('',(-3.5,-7.8,1.));
#12732=CARTESIAN_POINT('Origin',(3.5,-7.8,1.8));
#12733=CARTESIAN_POINT('',(3.5,-7.8,1.));
#12734=CARTESIAN_POINT('',(3.5,-7.8,1.));
#12735=CARTESIAN_POINT('',(3.5,-6.2,1.));
#12736=CARTESIAN_POINT('',(3.5,-7.8,1.));
#12737=CARTESIAN_POINT('',(3.5,-6.2,1.));
#12738=CARTESIAN_POINT('Origin',(-2.4,-7.8,1.));
#12739=CARTESIAN_POINT('',(2.4,-7.8,10.));
#12740=CARTESIAN_POINT('',(2.4,-7.8,1.));
#12741=CARTESIAN_POINT('',(-2.4,-7.8,10.));
#12742=CARTESIAN_POINT('',(-2.4,-7.8,10.));
#12743=CARTESIAN_POINT('',(-2.4,-7.8,1.));
#12744=CARTESIAN_POINT('',(-3.5,-7.8,1.));
#12745=CARTESIAN_POINT('Origin',(2.4,-7.8,1.));
#12746=CARTESIAN_POINT('',(2.4,-6.2,10.));
#12747=CARTESIAN_POINT('',(2.4,-6.2,1.));
#12748=CARTESIAN_POINT('',(2.4,-7.8,10.));
#12749=CARTESIAN_POINT('Origin',(2.4,-6.2,1.));
#12750=CARTESIAN_POINT('',(-2.4,-6.2,10.));
#12751=CARTESIAN_POINT('',(-2.4,-6.2,1.));
#12752=CARTESIAN_POINT('',(2.4,-6.2,10.));
#12753=CARTESIAN_POINT('',(-3.5,-6.2,1.));
#12754=CARTESIAN_POINT('Origin',(-2.4,-6.2,1.));
#12755=CARTESIAN_POINT('',(-2.4,-6.2,10.));
#12756=CARTESIAN_POINT('Origin',(0.,-7.,10.));
#12757=CARTESIAN_POINT('Origin',(0.,-7.,1.));
#12758=CARTESIAN_POINT('',(0.,0.,0.));
#12759=CARTESIAN_POINT('Origin',(-1.48492424049175,-8.1,5.51507575950825));
#12760=CARTESIAN_POINT('',(-1.70992424049175,-8.,5.51507575950825));
#12761=CARTESIAN_POINT('Origin',(-1.48492424049175,-8.,5.51507575950825));
#12762=CARTESIAN_POINT('',(-1.70992424049175,-7.8,5.51507575950825));
#12763=CARTESIAN_POINT('',(-1.70992424049175,-8.1,5.51507575950825));
#12764=CARTESIAN_POINT('Origin',(-1.48492424049175,-7.8,5.51507575950825));
#12765=CARTESIAN_POINT('Origin',(-1.48492424049175,-8.1,8.48492424049175));
#12766=CARTESIAN_POINT('',(-1.70992424049175,-8.,8.48492424049175));
#12767=CARTESIAN_POINT('Origin',(-1.48492424049175,-8.,8.48492424049175));
#12768=CARTESIAN_POINT('',(-1.70992424049175,-7.8,8.48492424049175));
#12769=CARTESIAN_POINT('',(-1.70992424049175,-8.1,8.48492424049175));
#12770=CARTESIAN_POINT('Origin',(-1.48492424049175,-7.8,8.48492424049175));
#12771=CARTESIAN_POINT('Origin',(1.48492424049175,-8.1,8.48492424049175));
#12772=CARTESIAN_POINT('',(1.25992424049175,-8.,8.48492424049175));
#12773=CARTESIAN_POINT('Origin',(1.48492424049175,-8.,8.48492424049175));
#12774=CARTESIAN_POINT('',(1.25992424049175,-7.8,8.48492424049175));
#12775=CARTESIAN_POINT('',(1.25992424049175,-8.1,8.48492424049175));
#12776=CARTESIAN_POINT('Origin',(1.48492424049175,-7.8,8.48492424049175));
#12777=CARTESIAN_POINT('Origin',(1.48492424049175,-8.1,5.51507575950825));
#12778=CARTESIAN_POINT('',(1.25992424049175,-8.,5.51507575950825));
#12779=CARTESIAN_POINT('Origin',(1.48492424049175,-8.,5.51507575950825));
#12780=CARTESIAN_POINT('',(1.25992424049175,-7.8,5.51507575950825));
#12781=CARTESIAN_POINT('',(1.25992424049175,-8.1,5.51507575950825));
#12782=CARTESIAN_POINT('Origin',(1.48492424049175,-7.8,5.51507575950825));
#12783=CARTESIAN_POINT('Origin',(0.,-7.8,7.));
#12784=CARTESIAN_POINT('',(-1.59,-7.5,7.));
#12785=CARTESIAN_POINT('Origin',(0.,-7.5,7.));
#12786=CARTESIAN_POINT('',(-1.59,-7.8,7.));
#12787=CARTESIAN_POINT('',(-1.59,-7.8,7.));
#12788=CARTESIAN_POINT('Origin',(0.,-7.8,7.));
#12789=CARTESIAN_POINT('Origin',(0.,-7.5,7.));
#12790=CARTESIAN_POINT('',(-1.2,-7.5,7.));
#12791=CARTESIAN_POINT('Origin',(0.,-7.5,7.));
#12792=CARTESIAN_POINT('Origin',(0.,-8.,7.));
#12793=CARTESIAN_POINT('',(-1.2,-8.,7.));
#12794=CARTESIAN_POINT('',(-1.2,-8.,7.));
#12795=CARTESIAN_POINT('Origin',(0.,-8.,7.));
#12796=CARTESIAN_POINT('Origin',(0.,-8.,7.));
#12797=CARTESIAN_POINT('',(-2.4,-7.8,7.));
#12798=CARTESIAN_POINT('Origin',(0.,-7.8,7.));
#12799=CARTESIAN_POINT('',(-2.4,-8.,7.));
#12800=CARTESIAN_POINT('',(-2.4,-8.,7.));
#12801=CARTESIAN_POINT('Origin',(0.,-8.,7.));
#12802=CARTESIAN_POINT('Origin',(0.,-7.8,7.));
#12803=CARTESIAN_POINT('Origin',(0.,-8.,7.));
#12804=CARTESIAN_POINT('',(0.,0.,0.));
#12805=CARTESIAN_POINT('Origin',(-1.48492424049175,-6.3,5.51507575950825));
#12806=CARTESIAN_POINT('',(-1.70992424049175,-6.2,5.51507575950825));
#12807=CARTESIAN_POINT('Origin',(-1.48492424049175,-6.2,5.51507575950825));
#12808=CARTESIAN_POINT('',(-1.70992424049175,-6.,5.51507575950825));
#12809=CARTESIAN_POINT('',(-1.70992424049175,-6.3,5.51507575950825));
#12810=CARTESIAN_POINT('Origin',(-1.48492424049175,-6.,5.51507575950825));
#12811=CARTESIAN_POINT('Origin',(-1.48492424049175,-6.3,8.48492424049175));
#12812=CARTESIAN_POINT('',(-1.70992424049175,-6.2,8.48492424049175));
#12813=CARTESIAN_POINT('Origin',(-1.48492424049175,-6.2,8.48492424049175));
#12814=CARTESIAN_POINT('',(-1.70992424049175,-6.,8.48492424049175));
#12815=CARTESIAN_POINT('',(-1.70992424049175,-6.3,8.48492424049175));
#12816=CARTESIAN_POINT('Origin',(-1.48492424049175,-6.,8.48492424049175));
#12817=CARTESIAN_POINT('Origin',(1.48492424049175,-6.3,8.48492424049175));
#12818=CARTESIAN_POINT('',(1.25992424049175,-6.2,8.48492424049175));
#12819=CARTESIAN_POINT('Origin',(1.48492424049175,-6.2,8.48492424049175));
#12820=CARTESIAN_POINT('',(1.25992424049175,-6.,8.48492424049175));
#12821=CARTESIAN_POINT('',(1.25992424049175,-6.3,8.48492424049175));
#12822=CARTESIAN_POINT('Origin',(1.48492424049175,-6.,8.48492424049175));
#12823=CARTESIAN_POINT('Origin',(1.48492424049175,-6.3,5.51507575950825));
#12824=CARTESIAN_POINT('',(1.25992424049175,-6.2,5.51507575950825));
#12825=CARTESIAN_POINT('Origin',(1.48492424049175,-6.2,5.51507575950825));
#12826=CARTESIAN_POINT('',(1.25992424049175,-6.,5.51507575950825));
#12827=CARTESIAN_POINT('',(1.25992424049175,-6.3,5.51507575950825));
#12828=CARTESIAN_POINT('Origin',(1.48492424049175,-6.,5.51507575950825));
#12829=CARTESIAN_POINT('Origin',(0.,-6.5,7.));
#12830=CARTESIAN_POINT('',(-1.59,-6.2,7.));
#12831=CARTESIAN_POINT('Origin',(0.,-6.2,7.));
#12832=CARTESIAN_POINT('',(-1.59,-6.5,7.));
#12833=CARTESIAN_POINT('',(-1.59,-6.5,7.));
#12834=CARTESIAN_POINT('Origin',(0.,-6.5,7.));
#12835=CARTESIAN_POINT('Origin',(0.,-6.5,7.));
#12836=CARTESIAN_POINT('',(-1.2,-6.5,7.));
#12837=CARTESIAN_POINT('Origin',(0.,-6.5,7.));
#12838=CARTESIAN_POINT('Origin',(0.,-6.2,7.));
#12839=CARTESIAN_POINT('',(-1.2,-6.,7.));
#12840=CARTESIAN_POINT('Origin',(0.,-6.,7.));
#12841=CARTESIAN_POINT('',(-1.2,-6.2,7.));
#12842=CARTESIAN_POINT('Origin',(0.,-6.2,7.));
#12843=CARTESIAN_POINT('',(-2.4,-6.,7.));
#12844=CARTESIAN_POINT('Origin',(0.,-6.,7.));
#12845=CARTESIAN_POINT('',(-2.4,-6.2,7.));
#12846=CARTESIAN_POINT('',(-2.4,-6.2,7.));
#12847=CARTESIAN_POINT('Origin',(0.,-6.2,7.));
#12848=CARTESIAN_POINT('Origin',(0.,-6.,7.));
#12849=CARTESIAN_POINT('Origin',(0.,-6.2,7.));
#12850=CARTESIAN_POINT('',(0.,0.,0.));
#12851=CARTESIAN_POINT('Origin',(-1.48492424049175,-4.9,5.51507575950825));
#12852=CARTESIAN_POINT('',(-1.64992424049175,-4.8,5.51507575950825));
#12853=CARTESIAN_POINT('Origin',(-1.48492424049175,-4.8,5.51507575950825));
#12854=CARTESIAN_POINT('',(-1.64992424049175,-3.2,5.51507575950825));
#12855=CARTESIAN_POINT('',(-1.64992424049175,-4.9,5.51507575950825));
#12856=CARTESIAN_POINT('Origin',(-1.48492424049175,-3.2,5.51507575950825));
#12857=CARTESIAN_POINT('Origin',(-1.48492424049175,-4.9,8.48492424049175));
#12858=CARTESIAN_POINT('',(-1.64992424049175,-4.8,8.48492424049175));
#12859=CARTESIAN_POINT('Origin',(-1.48492424049175,-4.8,8.48492424049175));
#12860=CARTESIAN_POINT('',(-1.64992424049175,-3.2,8.48492424049175));
#12861=CARTESIAN_POINT('',(-1.64992424049175,-4.9,8.48492424049175));
#12862=CARTESIAN_POINT('Origin',(-1.48492424049175,-3.2,8.48492424049175));
#12863=CARTESIAN_POINT('Origin',(1.48492424049175,-4.9,8.48492424049175));
#12864=CARTESIAN_POINT('',(1.31992424049175,-4.8,8.48492424049175));
#12865=CARTESIAN_POINT('Origin',(1.48492424049175,-4.8,8.48492424049175));
#12866=CARTESIAN_POINT('',(1.31992424049175,-3.2,8.48492424049175));
#12867=CARTESIAN_POINT('',(1.31992424049175,-4.9,8.48492424049175));
#12868=CARTESIAN_POINT('Origin',(1.48492424049175,-3.2,8.48492424049175));
#12869=CARTESIAN_POINT('Origin',(1.48492424049175,-4.9,5.51507575950825));
#12870=CARTESIAN_POINT('',(1.31992424049175,-4.8,5.51507575950825));
#12871=CARTESIAN_POINT('Origin',(1.48492424049175,-4.8,5.51507575950825));
#12872=CARTESIAN_POINT('',(1.31992424049175,-3.2,5.51507575950825));
#12873=CARTESIAN_POINT('',(1.31992424049175,-4.9,5.51507575950825));
#12874=CARTESIAN_POINT('Origin',(1.48492424049175,-3.2,5.51507575950825));
#12875=CARTESIAN_POINT('Origin',(0.,-4.9,7.));
#12876=CARTESIAN_POINT('',(-1.6,-4.8,7.));
#12877=CARTESIAN_POINT('Origin',(0.,-4.8,7.));
#12878=CARTESIAN_POINT('',(-1.6,-3.2,7.));
#12879=CARTESIAN_POINT('',(-1.6,-4.9,7.));
#12880=CARTESIAN_POINT('Origin',(0.,-3.2,7.));
#12881=CARTESIAN_POINT('Origin',(-2.9,-4.,0.9));
#12882=CARTESIAN_POINT('',(-3.125,-4.,1.));
#12883=CARTESIAN_POINT('Origin',(-2.9,-4.,1.));
#12884=CARTESIAN_POINT('',(-3.125,-4.,1.8));
#12885=CARTESIAN_POINT('',(-3.125,-4.,0.9));
#12886=CARTESIAN_POINT('Origin',(-2.9,-4.,1.8));
#12887=CARTESIAN_POINT('Origin',(2.9,-4.,0.9));
#12888=CARTESIAN_POINT('',(2.675,-4.,1.));
#12889=CARTESIAN_POINT('Origin',(2.9,-4.,1.));
#12890=CARTESIAN_POINT('',(2.675,-4.,1.8));
#12891=CARTESIAN_POINT('',(2.675,-4.,0.9));
#12892=CARTESIAN_POINT('Origin',(2.9,-4.,1.8));
#12893=CARTESIAN_POINT('Origin',(-3.5,-4.8,1.8));
#12894=CARTESIAN_POINT('',(2.4,-4.8,1.8));
#12895=CARTESIAN_POINT('',(2.4,-3.2,1.8));
#12896=CARTESIAN_POINT('',(2.4,-4.8,1.8));
#12897=CARTESIAN_POINT('',(3.5,-4.8,1.8));
#12898=CARTESIAN_POINT('',(3.5,-4.8,1.8));
#12899=CARTESIAN_POINT('',(3.5,-3.2,1.8));
#12900=CARTESIAN_POINT('',(3.5,-4.8,1.8));
#12901=CARTESIAN_POINT('',(3.5,-3.2,1.8));
#12902=CARTESIAN_POINT('Origin',(-3.5,-4.8,1.8));
#12903=CARTESIAN_POINT('',(-2.4,-3.2,1.8));
#12904=CARTESIAN_POINT('',(-2.4,-4.8,1.8));
#12905=CARTESIAN_POINT('',(-2.4,-4.,1.8));
#12906=CARTESIAN_POINT('',(-3.5,-3.2,1.8));
#12907=CARTESIAN_POINT('',(3.5,-3.2,1.8));
#12908=CARTESIAN_POINT('',(-3.5,-4.8,1.8));
#12909=CARTESIAN_POINT('',(-3.5,-4.8,1.8));
#12910=CARTESIAN_POINT('',(3.5,-4.8,1.8));
#12911=CARTESIAN_POINT('Origin',(-3.5,-4.8,1.));
#12912=CARTESIAN_POINT('',(-3.5,-4.8,1.));
#12913=CARTESIAN_POINT('',(-3.5,-4.8,1.8));
#12914=CARTESIAN_POINT('',(-3.5,-3.2,1.));
#12915=CARTESIAN_POINT('',(-3.5,-3.2,1.8));
#12916=CARTESIAN_POINT('',(-3.5,-4.8,1.));
#12917=CARTESIAN_POINT('Origin',(3.5,-4.8,1.8));
#12918=CARTESIAN_POINT('',(3.5,-4.8,1.));
#12919=CARTESIAN_POINT('',(3.5,-4.8,1.));
#12920=CARTESIAN_POINT('',(3.5,-3.2,1.));
#12921=CARTESIAN_POINT('',(3.5,-4.8,1.));
#12922=CARTESIAN_POINT('',(3.5,-3.2,1.));
#12923=CARTESIAN_POINT('Origin',(-2.4,-4.8,1.));
#12924=CARTESIAN_POINT('',(2.4,-4.8,10.));
#12925=CARTESIAN_POINT('',(2.4,-4.8,1.));
#12926=CARTESIAN_POINT('',(-2.4,-4.8,10.));
#12927=CARTESIAN_POINT('',(-2.4,-4.8,10.));
#12928=CARTESIAN_POINT('',(-2.4,-4.8,1.));
#12929=CARTESIAN_POINT('',(-3.5,-4.8,1.));
#12930=CARTESIAN_POINT('Origin',(2.4,-4.8,1.));
#12931=CARTESIAN_POINT('',(2.4,-3.2,10.));
#12932=CARTESIAN_POINT('',(2.4,-3.2,1.));
#12933=CARTESIAN_POINT('',(2.4,-4.8,10.));
#12934=CARTESIAN_POINT('Origin',(2.4,-3.2,1.));
#12935=CARTESIAN_POINT('',(-2.4,-3.2,10.));
#12936=CARTESIAN_POINT('',(-2.4,-3.2,1.));
#12937=CARTESIAN_POINT('',(2.4,-3.2,10.));
#12938=CARTESIAN_POINT('',(-3.5,-3.2,1.));
#12939=CARTESIAN_POINT('Origin',(-2.4,-3.2,1.));
#12940=CARTESIAN_POINT('',(-2.4,-3.2,10.));
#12941=CARTESIAN_POINT('Origin',(0.,-4.,10.));
#12942=CARTESIAN_POINT('Origin',(0.,-4.,1.));
#12943=CARTESIAN_POINT('',(0.,0.,0.));
#12944=CARTESIAN_POINT('Origin',(-1.48492424049175,-5.1,5.51507575950825));
#12945=CARTESIAN_POINT('',(-1.70992424049175,-5.,5.51507575950825));
#12946=CARTESIAN_POINT('Origin',(-1.48492424049175,-5.,5.51507575950825));
#12947=CARTESIAN_POINT('',(-1.70992424049175,-4.8,5.51507575950825));
#12948=CARTESIAN_POINT('',(-1.70992424049175,-5.1,5.51507575950825));
#12949=CARTESIAN_POINT('Origin',(-1.48492424049175,-4.8,5.51507575950825));
#12950=CARTESIAN_POINT('Origin',(-1.48492424049175,-5.1,8.48492424049175));
#12951=CARTESIAN_POINT('',(-1.70992424049175,-5.,8.48492424049175));
#12952=CARTESIAN_POINT('Origin',(-1.48492424049175,-5.,8.48492424049175));
#12953=CARTESIAN_POINT('',(-1.70992424049175,-4.8,8.48492424049175));
#12954=CARTESIAN_POINT('',(-1.70992424049175,-5.1,8.48492424049175));
#12955=CARTESIAN_POINT('Origin',(-1.48492424049175,-4.8,8.48492424049175));
#12956=CARTESIAN_POINT('Origin',(1.48492424049175,-5.1,8.48492424049175));
#12957=CARTESIAN_POINT('',(1.25992424049175,-5.,8.48492424049175));
#12958=CARTESIAN_POINT('Origin',(1.48492424049175,-5.,8.48492424049175));
#12959=CARTESIAN_POINT('',(1.25992424049175,-4.8,8.48492424049175));
#12960=CARTESIAN_POINT('',(1.25992424049175,-5.1,8.48492424049175));
#12961=CARTESIAN_POINT('Origin',(1.48492424049175,-4.8,8.48492424049175));
#12962=CARTESIAN_POINT('Origin',(1.48492424049175,-5.1,5.51507575950825));
#12963=CARTESIAN_POINT('',(1.25992424049175,-5.,5.51507575950825));
#12964=CARTESIAN_POINT('Origin',(1.48492424049175,-5.,5.51507575950825));
#12965=CARTESIAN_POINT('',(1.25992424049175,-4.8,5.51507575950825));
#12966=CARTESIAN_POINT('',(1.25992424049175,-5.1,5.51507575950825));
#12967=CARTESIAN_POINT('Origin',(1.48492424049175,-4.8,5.51507575950825));
#12968=CARTESIAN_POINT('Origin',(0.,-4.8,7.));
#12969=CARTESIAN_POINT('',(-1.59,-4.5,7.));
#12970=CARTESIAN_POINT('Origin',(0.,-4.5,7.));
#12971=CARTESIAN_POINT('',(-1.59,-4.8,7.));
#12972=CARTESIAN_POINT('',(-1.59,-4.8,7.));
#12973=CARTESIAN_POINT('Origin',(0.,-4.8,7.));
#12974=CARTESIAN_POINT('Origin',(0.,-4.5,7.));
#12975=CARTESIAN_POINT('',(-1.2,-4.5,7.));
#12976=CARTESIAN_POINT('Origin',(0.,-4.5,7.));
#12977=CARTESIAN_POINT('Origin',(0.,-5.,7.));
#12978=CARTESIAN_POINT('',(-1.2,-5.,7.));
#12979=CARTESIAN_POINT('',(-1.2,-5.,7.));
#12980=CARTESIAN_POINT('Origin',(0.,-5.,7.));
#12981=CARTESIAN_POINT('Origin',(0.,-5.,7.));
#12982=CARTESIAN_POINT('',(-2.4,-4.8,7.));
#12983=CARTESIAN_POINT('Origin',(0.,-4.8,7.));
#12984=CARTESIAN_POINT('',(-2.4,-5.,7.));
#12985=CARTESIAN_POINT('',(-2.4,-5.,7.));
#12986=CARTESIAN_POINT('Origin',(0.,-5.,7.));
#12987=CARTESIAN_POINT('Origin',(0.,-4.8,7.));
#12988=CARTESIAN_POINT('Origin',(0.,-5.,7.));
#12989=CARTESIAN_POINT('',(0.,0.,0.));
#12990=CARTESIAN_POINT('Origin',(-1.48492424049175,-3.3,5.51507575950825));
#12991=CARTESIAN_POINT('',(-1.70992424049175,-3.2,5.51507575950825));
#12992=CARTESIAN_POINT('Origin',(-1.48492424049175,-3.2,5.51507575950825));
#12993=CARTESIAN_POINT('',(-1.70992424049175,-3.,5.51507575950825));
#12994=CARTESIAN_POINT('',(-1.70992424049175,-3.3,5.51507575950825));
#12995=CARTESIAN_POINT('Origin',(-1.48492424049175,-3.,5.51507575950825));
#12996=CARTESIAN_POINT('Origin',(-1.48492424049175,-3.3,8.48492424049175));
#12997=CARTESIAN_POINT('',(-1.70992424049175,-3.2,8.48492424049175));
#12998=CARTESIAN_POINT('Origin',(-1.48492424049175,-3.2,8.48492424049175));
#12999=CARTESIAN_POINT('',(-1.70992424049175,-3.,8.48492424049175));
#13000=CARTESIAN_POINT('',(-1.70992424049175,-3.3,8.48492424049175));
#13001=CARTESIAN_POINT('Origin',(-1.48492424049175,-3.,8.48492424049175));
#13002=CARTESIAN_POINT('Origin',(1.48492424049175,-3.3,8.48492424049175));
#13003=CARTESIAN_POINT('',(1.25992424049175,-3.2,8.48492424049175));
#13004=CARTESIAN_POINT('Origin',(1.48492424049175,-3.2,8.48492424049175));
#13005=CARTESIAN_POINT('',(1.25992424049175,-3.,8.48492424049175));
#13006=CARTESIAN_POINT('',(1.25992424049175,-3.3,8.48492424049175));
#13007=CARTESIAN_POINT('Origin',(1.48492424049175,-3.,8.48492424049175));
#13008=CARTESIAN_POINT('Origin',(1.48492424049175,-3.3,5.51507575950825));
#13009=CARTESIAN_POINT('',(1.25992424049175,-3.2,5.51507575950825));
#13010=CARTESIAN_POINT('Origin',(1.48492424049175,-3.2,5.51507575950825));
#13011=CARTESIAN_POINT('',(1.25992424049175,-3.,5.51507575950825));
#13012=CARTESIAN_POINT('',(1.25992424049175,-3.3,5.51507575950825));
#13013=CARTESIAN_POINT('Origin',(1.48492424049175,-3.,5.51507575950825));
#13014=CARTESIAN_POINT('Origin',(0.,-3.5,7.));
#13015=CARTESIAN_POINT('',(-1.59,-3.2,7.));
#13016=CARTESIAN_POINT('Origin',(0.,-3.2,7.));
#13017=CARTESIAN_POINT('',(-1.59,-3.5,7.));
#13018=CARTESIAN_POINT('',(-1.59,-3.5,7.));
#13019=CARTESIAN_POINT('Origin',(0.,-3.5,7.));
#13020=CARTESIAN_POINT('Origin',(0.,-3.5,7.));
#13021=CARTESIAN_POINT('',(-1.2,-3.5,7.));
#13022=CARTESIAN_POINT('Origin',(0.,-3.5,7.));
#13023=CARTESIAN_POINT('Origin',(0.,-3.2,7.));
#13024=CARTESIAN_POINT('',(-1.2,-3.,7.));
#13025=CARTESIAN_POINT('Origin',(0.,-3.,7.));
#13026=CARTESIAN_POINT('',(-1.2,-3.2,7.));
#13027=CARTESIAN_POINT('Origin',(0.,-3.2,7.));
#13028=CARTESIAN_POINT('',(-2.4,-3.,7.));
#13029=CARTESIAN_POINT('Origin',(0.,-3.,7.));
#13030=CARTESIAN_POINT('',(-2.4,-3.2,7.));
#13031=CARTESIAN_POINT('',(-2.4,-3.2,7.));
#13032=CARTESIAN_POINT('Origin',(0.,-3.2,7.));
#13033=CARTESIAN_POINT('Origin',(0.,-3.,7.));
#13034=CARTESIAN_POINT('Origin',(0.,-3.2,7.));
#13035=CARTESIAN_POINT('',(0.,0.,0.));
#13036=CARTESIAN_POINT('Origin',(-1.2,1.51507575950825,5.51507575950825));
#13037=CARTESIAN_POINT('',(-1.1,1.51507575950825,5.68007575950825));
#13038=CARTESIAN_POINT('Origin',(-1.1,1.51507575950825,5.51507575950825));
#13039=CARTESIAN_POINT('',(0.5,1.51507575950825,5.68007575950825));
#13040=CARTESIAN_POINT('',(-1.2,1.51507575950825,5.68007575950825));
#13041=CARTESIAN_POINT('Origin',(0.5,1.51507575950825,5.51507575950825));
#13042=CARTESIAN_POINT('Origin',(-1.2,1.51507575950825,8.48492424049175));
#13043=CARTESIAN_POINT('',(-1.1,1.51507575950825,8.64992424049175));
#13044=CARTESIAN_POINT('Origin',(-1.1,1.51507575950825,8.48492424049175));
#13045=CARTESIAN_POINT('',(0.5,1.51507575950825,8.64992424049175));
#13046=CARTESIAN_POINT('',(-1.2,1.51507575950825,8.64992424049175));
#13047=CARTESIAN_POINT('Origin',(0.5,1.51507575950825,8.48492424049175));
#13048=CARTESIAN_POINT('Origin',(-1.2,4.48492424049175,8.48492424049175));
#13049=CARTESIAN_POINT('',(-1.1,4.48492424049175,8.64992424049175));
#13050=CARTESIAN_POINT('Origin',(-1.1,4.48492424049175,8.48492424049175));
#13051=CARTESIAN_POINT('',(0.5,4.48492424049175,8.64992424049175));
#13052=CARTESIAN_POINT('',(-1.2,4.48492424049175,8.64992424049175));
#13053=CARTESIAN_POINT('Origin',(0.5,4.48492424049175,8.48492424049175));
#13054=CARTESIAN_POINT('Origin',(-1.2,4.48492424049175,5.51507575950825));
#13055=CARTESIAN_POINT('',(-1.1,4.48492424049175,5.68007575950825));
#13056=CARTESIAN_POINT('Origin',(-1.1,4.48492424049175,5.51507575950825));
#13057=CARTESIAN_POINT('',(0.5,4.48492424049175,5.68007575950825));
#13058=CARTESIAN_POINT('',(-1.2,4.48492424049175,5.68007575950825));
#13059=CARTESIAN_POINT('Origin',(0.5,4.48492424049175,5.51507575950825));
#13060=CARTESIAN_POINT('Origin',(-1.2,3.,7.));
#13061=CARTESIAN_POINT('',(-1.1,3.,8.6));
#13062=CARTESIAN_POINT('Origin',(-1.1,3.,7.));
#13063=CARTESIAN_POINT('',(0.5,3.,8.6));
#13064=CARTESIAN_POINT('',(-1.2,3.,8.6));
#13065=CARTESIAN_POINT('Origin',(0.5,3.,7.));
#13066=CARTESIAN_POINT('Origin',(-1.7,1.5,1.9));
#13067=CARTESIAN_POINT('',(-1.925,1.5,2.));
#13068=CARTESIAN_POINT('Origin',(-1.7,1.5,2.));
#13069=CARTESIAN_POINT('',(-1.925,1.5,2.8));
#13070=CARTESIAN_POINT('',(-1.925,1.5,1.9));
#13071=CARTESIAN_POINT('Origin',(-1.7,1.5,2.8));
#13072=CARTESIAN_POINT('Origin',(1.1,4.5,1.9));
#13073=CARTESIAN_POINT('',(0.875,4.5,2.));
#13074=CARTESIAN_POINT('Origin',(1.1,4.5,2.));
#13075=CARTESIAN_POINT('',(0.875,4.5,2.8));
#13076=CARTESIAN_POINT('',(0.875,4.5,1.9));
#13077=CARTESIAN_POINT('Origin',(1.1,4.5,2.8));
#13078=CARTESIAN_POINT('Origin',(-2.2,0.6,2.8));
#13079=CARTESIAN_POINT('',(0.5,0.6,2.8));
#13080=CARTESIAN_POINT('',(0.5,5.4,2.8));
#13081=CARTESIAN_POINT('',(0.5,0.6,2.8));
#13082=CARTESIAN_POINT('',(1.6,0.6,2.8));
#13083=CARTESIAN_POINT('',(1.6,0.6,2.8));
#13084=CARTESIAN_POINT('',(1.6,5.4,2.8));
#13085=CARTESIAN_POINT('',(1.6,0.6,2.8));
#13086=CARTESIAN_POINT('',(1.6,5.4,2.8));
#13087=CARTESIAN_POINT('Origin',(-2.2,0.6,2.8));
#13088=CARTESIAN_POINT('',(-1.1,5.4,2.8));
#13089=CARTESIAN_POINT('',(-1.1,0.6,2.8));
#13090=CARTESIAN_POINT('',(-1.1,3.,2.8));
#13091=CARTESIAN_POINT('',(-2.2,5.4,2.8));
#13092=CARTESIAN_POINT('',(1.6,5.4,2.8));
#13093=CARTESIAN_POINT('',(-2.2,0.6,2.8));
#13094=CARTESIAN_POINT('',(-2.2,0.6,2.8));
#13095=CARTESIAN_POINT('',(1.6,0.6,2.8));
#13096=CARTESIAN_POINT('Origin',(-2.2,0.6,2.));
#13097=CARTESIAN_POINT('',(-2.2,0.6,2.));
#13098=CARTESIAN_POINT('',(-2.2,0.6,2.8));
#13099=CARTESIAN_POINT('',(-2.2,5.4,2.));
#13100=CARTESIAN_POINT('',(-2.2,5.4,2.8));
#13101=CARTESIAN_POINT('',(-2.2,0.6,2.));
#13102=CARTESIAN_POINT('Origin',(1.6,0.6,2.8));
#13103=CARTESIAN_POINT('',(1.6,0.6,2.));
#13104=CARTESIAN_POINT('',(1.6,0.6,2.));
#13105=CARTESIAN_POINT('',(1.6,5.4,2.));
#13106=CARTESIAN_POINT('',(1.6,0.6,2.));
#13107=CARTESIAN_POINT('',(1.6,5.4,2.));
#13108=CARTESIAN_POINT('Origin',(-1.1,0.6,2.));
#13109=CARTESIAN_POINT('',(0.5,0.6,10.));
#13110=CARTESIAN_POINT('',(0.5,0.6,2.));
#13111=CARTESIAN_POINT('',(-1.1,0.6,10.));
#13112=CARTESIAN_POINT('',(-1.1,0.6,10.));
#13113=CARTESIAN_POINT('',(-1.1,0.6,2.));
#13114=CARTESIAN_POINT('',(-2.2,0.6,2.));
#13115=CARTESIAN_POINT('Origin',(0.5,0.6,2.));
#13116=CARTESIAN_POINT('',(0.5,5.4,10.));
#13117=CARTESIAN_POINT('',(0.5,5.4,2.));
#13118=CARTESIAN_POINT('',(0.5,0.6,10.));
#13119=CARTESIAN_POINT('Origin',(0.5,5.4,2.));
#13120=CARTESIAN_POINT('',(-1.1,5.4,10.));
#13121=CARTESIAN_POINT('',(-1.1,5.4,2.));
#13122=CARTESIAN_POINT('',(0.5,5.4,10.));
#13123=CARTESIAN_POINT('',(-2.2,5.4,2.));
#13124=CARTESIAN_POINT('Origin',(-1.1,5.4,2.));
#13125=CARTESIAN_POINT('',(-1.1,5.4,10.));
#13126=CARTESIAN_POINT('Origin',(-0.3,3.,10.));
#13127=CARTESIAN_POINT('Origin',(-0.3,3.,2.));
#13128=CARTESIAN_POINT('',(0.,0.,0.));
#13129=CARTESIAN_POINT('Origin',(-1.4,1.51507575950825,5.51507575950825));
#13130=CARTESIAN_POINT('',(-1.3,1.51507575950825,5.74007575950825));
#13131=CARTESIAN_POINT('Origin',(-1.3,1.51507575950825,5.51507575950825));
#13132=CARTESIAN_POINT('',(-1.1,1.51507575950825,5.74007575950825));
#13133=CARTESIAN_POINT('',(-1.4,1.51507575950825,5.74007575950825));
#13134=CARTESIAN_POINT('Origin',(-1.1,1.51507575950825,5.51507575950825));
#13135=CARTESIAN_POINT('Origin',(-1.4,1.51507575950825,8.48492424049175));
#13136=CARTESIAN_POINT('',(-1.3,1.51507575950825,8.70992424049175));
#13137=CARTESIAN_POINT('Origin',(-1.3,1.51507575950825,8.48492424049175));
#13138=CARTESIAN_POINT('',(-1.1,1.51507575950825,8.70992424049175));
#13139=CARTESIAN_POINT('',(-1.4,1.51507575950825,8.70992424049175));
#13140=CARTESIAN_POINT('Origin',(-1.1,1.51507575950825,8.48492424049175));
#13141=CARTESIAN_POINT('Origin',(-1.4,4.48492424049175,8.48492424049175));
#13142=CARTESIAN_POINT('',(-1.3,4.48492424049175,8.70992424049175));
#13143=CARTESIAN_POINT('Origin',(-1.3,4.48492424049175,8.48492424049175));
#13144=CARTESIAN_POINT('',(-1.1,4.48492424049175,8.70992424049175));
#13145=CARTESIAN_POINT('',(-1.4,4.48492424049175,8.70992424049175));
#13146=CARTESIAN_POINT('Origin',(-1.1,4.48492424049175,8.48492424049175));
#13147=CARTESIAN_POINT('Origin',(-1.4,4.48492424049175,5.51507575950825));
#13148=CARTESIAN_POINT('',(-1.3,4.48492424049175,5.74007575950825));
#13149=CARTESIAN_POINT('Origin',(-1.3,4.48492424049175,5.51507575950825));
#13150=CARTESIAN_POINT('',(-1.1,4.48492424049175,5.74007575950825));
#13151=CARTESIAN_POINT('',(-1.4,4.48492424049175,5.74007575950825));
#13152=CARTESIAN_POINT('Origin',(-1.1,4.48492424049175,5.51507575950825));
#13153=CARTESIAN_POINT('Origin',(-1.1,3.,7.));
#13154=CARTESIAN_POINT('',(-0.8,3.,8.59));
#13155=CARTESIAN_POINT('Origin',(-0.8,3.,7.));
#13156=CARTESIAN_POINT('',(-1.1,3.,8.59));
#13157=CARTESIAN_POINT('',(-1.1,3.,8.59));
#13158=CARTESIAN_POINT('Origin',(-1.1,3.,7.));
#13159=CARTESIAN_POINT('Origin',(-0.8,3.,7.));
#13160=CARTESIAN_POINT('',(-0.8,3.,8.2));
#13161=CARTESIAN_POINT('Origin',(-0.8,3.,7.));
#13162=CARTESIAN_POINT('Origin',(-1.3,3.,7.));
#13163=CARTESIAN_POINT('',(-1.3,3.,8.2));
#13164=CARTESIAN_POINT('',(-1.3,3.,8.2));
#13165=CARTESIAN_POINT('Origin',(-1.3,3.,7.));
#13166=CARTESIAN_POINT('Origin',(-1.3,3.,7.));
#13167=CARTESIAN_POINT('',(-1.1,3.,9.4));
#13168=CARTESIAN_POINT('Origin',(-1.1,3.,7.));
#13169=CARTESIAN_POINT('',(-1.3,3.,9.4));
#13170=CARTESIAN_POINT('',(-1.3,3.,9.4));
#13171=CARTESIAN_POINT('Origin',(-1.3,3.,7.));
#13172=CARTESIAN_POINT('Origin',(-1.1,3.,7.));
#13173=CARTESIAN_POINT('Origin',(-1.3,3.,7.));
#13174=CARTESIAN_POINT('',(0.,0.,0.));
#13175=CARTESIAN_POINT('Origin',(0.4,1.51507575950825,5.51507575950825));
#13176=CARTESIAN_POINT('',(0.5,1.51507575950825,5.74007575950825));
#13177=CARTESIAN_POINT('Origin',(0.5,1.51507575950825,5.51507575950825));
#13178=CARTESIAN_POINT('',(0.7,1.51507575950825,5.74007575950825));
#13179=CARTESIAN_POINT('',(0.4,1.51507575950825,5.74007575950825));
#13180=CARTESIAN_POINT('Origin',(0.7,1.51507575950825,5.51507575950825));
#13181=CARTESIAN_POINT('Origin',(0.4,1.51507575950825,8.48492424049175));
#13182=CARTESIAN_POINT('',(0.5,1.51507575950825,8.70992424049175));
#13183=CARTESIAN_POINT('Origin',(0.5,1.51507575950825,8.48492424049175));
#13184=CARTESIAN_POINT('',(0.7,1.51507575950825,8.70992424049175));
#13185=CARTESIAN_POINT('',(0.4,1.51507575950825,8.70992424049175));
#13186=CARTESIAN_POINT('Origin',(0.7,1.51507575950825,8.48492424049175));
#13187=CARTESIAN_POINT('Origin',(0.4,4.48492424049175,8.48492424049175));
#13188=CARTESIAN_POINT('',(0.5,4.48492424049175,8.70992424049175));
#13189=CARTESIAN_POINT('Origin',(0.5,4.48492424049175,8.48492424049175));
#13190=CARTESIAN_POINT('',(0.7,4.48492424049175,8.70992424049175));
#13191=CARTESIAN_POINT('',(0.4,4.48492424049175,8.70992424049175));
#13192=CARTESIAN_POINT('Origin',(0.7,4.48492424049175,8.48492424049175));
#13193=CARTESIAN_POINT('Origin',(0.4,4.48492424049175,5.51507575950825));
#13194=CARTESIAN_POINT('',(0.5,4.48492424049175,5.74007575950825));
#13195=CARTESIAN_POINT('Origin',(0.5,4.48492424049175,5.51507575950825));
#13196=CARTESIAN_POINT('',(0.7,4.48492424049175,5.74007575950825));
#13197=CARTESIAN_POINT('',(0.4,4.48492424049175,5.74007575950825));
#13198=CARTESIAN_POINT('Origin',(0.7,4.48492424049175,5.51507575950825));
#13199=CARTESIAN_POINT('Origin',(0.2,3.,7.));
#13200=CARTESIAN_POINT('',(0.5,3.,8.59));
#13201=CARTESIAN_POINT('Origin',(0.5,3.,7.));
#13202=CARTESIAN_POINT('',(0.2,3.,8.59));
#13203=CARTESIAN_POINT('',(0.2,3.,8.59));
#13204=CARTESIAN_POINT('Origin',(0.2,3.,7.));
#13205=CARTESIAN_POINT('Origin',(0.2,3.,7.));
#13206=CARTESIAN_POINT('',(0.2,3.,8.2));
#13207=CARTESIAN_POINT('Origin',(0.2,3.,7.));
#13208=CARTESIAN_POINT('Origin',(0.5,3.,7.));
#13209=CARTESIAN_POINT('',(0.7,3.,8.2));
#13210=CARTESIAN_POINT('Origin',(0.7,3.,7.));
#13211=CARTESIAN_POINT('',(0.5,3.,8.2));
#13212=CARTESIAN_POINT('Origin',(0.5,3.,7.));
#13213=CARTESIAN_POINT('',(0.7,3.,9.4));
#13214=CARTESIAN_POINT('Origin',(0.7,3.,7.));
#13215=CARTESIAN_POINT('',(0.5,3.,9.4));
#13216=CARTESIAN_POINT('',(0.5,3.,9.4));
#13217=CARTESIAN_POINT('Origin',(0.5,3.,7.));
#13218=CARTESIAN_POINT('Origin',(0.7,3.,7.));
#13219=CARTESIAN_POINT('Origin',(0.5,3.,7.));
#13220=CARTESIAN_POINT('',(0.,0.,0.));
#13221=CARTESIAN_POINT('Origin',(4.6,1.51507575950825,5.51507575950825));
#13222=CARTESIAN_POINT('',(4.7,1.51507575950825,5.68007575950825));
#13223=CARTESIAN_POINT('Origin',(4.7,1.51507575950825,5.51507575950825));
#13224=CARTESIAN_POINT('',(6.3,1.51507575950825,5.68007575950825));
#13225=CARTESIAN_POINT('',(4.6,1.51507575950825,5.68007575950825));
#13226=CARTESIAN_POINT('Origin',(6.3,1.51507575950825,5.51507575950825));
#13227=CARTESIAN_POINT('Origin',(4.6,1.51507575950825,8.48492424049175));
#13228=CARTESIAN_POINT('',(4.7,1.51507575950825,8.64992424049175));
#13229=CARTESIAN_POINT('Origin',(4.7,1.51507575950825,8.48492424049175));
#13230=CARTESIAN_POINT('',(6.3,1.51507575950825,8.64992424049175));
#13231=CARTESIAN_POINT('',(4.6,1.51507575950825,8.64992424049175));
#13232=CARTESIAN_POINT('Origin',(6.3,1.51507575950825,8.48492424049175));
#13233=CARTESIAN_POINT('Origin',(4.6,4.48492424049175,8.48492424049175));
#13234=CARTESIAN_POINT('',(4.7,4.48492424049175,8.64992424049175));
#13235=CARTESIAN_POINT('Origin',(4.7,4.48492424049175,8.48492424049175));
#13236=CARTESIAN_POINT('',(6.3,4.48492424049175,8.64992424049175));
#13237=CARTESIAN_POINT('',(4.6,4.48492424049175,8.64992424049175));
#13238=CARTESIAN_POINT('Origin',(6.3,4.48492424049175,8.48492424049175));
#13239=CARTESIAN_POINT('Origin',(4.6,4.48492424049175,5.51507575950825));
#13240=CARTESIAN_POINT('',(4.7,4.48492424049175,5.68007575950825));
#13241=CARTESIAN_POINT('Origin',(4.7,4.48492424049175,5.51507575950825));
#13242=CARTESIAN_POINT('',(6.3,4.48492424049175,5.68007575950825));
#13243=CARTESIAN_POINT('',(4.6,4.48492424049175,5.68007575950825));
#13244=CARTESIAN_POINT('Origin',(6.3,4.48492424049175,5.51507575950825));
#13245=CARTESIAN_POINT('Origin',(4.6,3.,7.));
#13246=CARTESIAN_POINT('',(4.7,3.,8.6));
#13247=CARTESIAN_POINT('Origin',(4.7,3.,7.));
#13248=CARTESIAN_POINT('',(6.3,3.,8.6));
#13249=CARTESIAN_POINT('',(4.6,3.,8.6));
#13250=CARTESIAN_POINT('Origin',(6.3,3.,7.));
#13251=CARTESIAN_POINT('Origin',(4.1,1.5,1.9));
#13252=CARTESIAN_POINT('',(3.875,1.5,2.));
#13253=CARTESIAN_POINT('Origin',(4.1,1.5,2.));
#13254=CARTESIAN_POINT('',(3.875,1.5,2.8));
#13255=CARTESIAN_POINT('',(3.875,1.5,1.9));
#13256=CARTESIAN_POINT('Origin',(4.1,1.5,2.8));
#13257=CARTESIAN_POINT('Origin',(6.9,4.5,1.9));
#13258=CARTESIAN_POINT('',(6.675,4.5,2.));
#13259=CARTESIAN_POINT('Origin',(6.9,4.5,2.));
#13260=CARTESIAN_POINT('',(6.675,4.5,2.8));
#13261=CARTESIAN_POINT('',(6.675,4.5,1.9));
#13262=CARTESIAN_POINT('Origin',(6.9,4.5,2.8));
#13263=CARTESIAN_POINT('Origin',(3.6,0.6,2.8));
#13264=CARTESIAN_POINT('',(6.3,0.6,2.8));
#13265=CARTESIAN_POINT('',(6.3,5.4,2.8));
#13266=CARTESIAN_POINT('',(6.3,0.6,2.8));
#13267=CARTESIAN_POINT('',(7.4,0.6,2.8));
#13268=CARTESIAN_POINT('',(7.4,0.6,2.8));
#13269=CARTESIAN_POINT('',(7.4,5.4,2.8));
#13270=CARTESIAN_POINT('',(7.4,0.6,2.8));
#13271=CARTESIAN_POINT('',(7.4,5.4,2.8));
#13272=CARTESIAN_POINT('Origin',(3.6,0.6,2.8));
#13273=CARTESIAN_POINT('',(4.7,5.4,2.8));
#13274=CARTESIAN_POINT('',(4.7,0.6,2.8));
#13275=CARTESIAN_POINT('',(4.7,3.,2.8));
#13276=CARTESIAN_POINT('',(3.6,5.4,2.8));
#13277=CARTESIAN_POINT('',(7.4,5.4,2.8));
#13278=CARTESIAN_POINT('',(3.6,0.6,2.8));
#13279=CARTESIAN_POINT('',(3.6,0.6,2.8));
#13280=CARTESIAN_POINT('',(7.4,0.6,2.8));
#13281=CARTESIAN_POINT('Origin',(3.6,0.6,2.));
#13282=CARTESIAN_POINT('',(3.6,0.6,2.));
#13283=CARTESIAN_POINT('',(3.6,0.6,2.8));
#13284=CARTESIAN_POINT('',(3.6,5.4,2.));
#13285=CARTESIAN_POINT('',(3.6,5.4,2.8));
#13286=CARTESIAN_POINT('',(3.6,0.6,2.));
#13287=CARTESIAN_POINT('Origin',(7.4,0.6,2.8));
#13288=CARTESIAN_POINT('',(7.4,0.6,2.));
#13289=CARTESIAN_POINT('',(7.4,0.6,2.));
#13290=CARTESIAN_POINT('',(7.4,5.4,2.));
#13291=CARTESIAN_POINT('',(7.4,0.6,2.));
#13292=CARTESIAN_POINT('',(7.4,5.4,2.));
#13293=CARTESIAN_POINT('Origin',(4.7,0.6,2.));
#13294=CARTESIAN_POINT('',(6.3,0.6,10.));
#13295=CARTESIAN_POINT('',(6.3,0.6,2.));
#13296=CARTESIAN_POINT('',(4.7,0.6,10.));
#13297=CARTESIAN_POINT('',(4.7,0.6,10.));
#13298=CARTESIAN_POINT('',(4.7,0.6,2.));
#13299=CARTESIAN_POINT('',(3.6,0.6,2.));
#13300=CARTESIAN_POINT('Origin',(6.3,0.6,2.));
#13301=CARTESIAN_POINT('',(6.3,5.4,10.));
#13302=CARTESIAN_POINT('',(6.3,5.4,2.));
#13303=CARTESIAN_POINT('',(6.3,0.6,10.));
#13304=CARTESIAN_POINT('Origin',(6.3,5.4,2.));
#13305=CARTESIAN_POINT('',(4.7,5.4,10.));
#13306=CARTESIAN_POINT('',(4.7,5.4,2.));
#13307=CARTESIAN_POINT('',(6.3,5.4,10.));
#13308=CARTESIAN_POINT('',(3.6,5.4,2.));
#13309=CARTESIAN_POINT('Origin',(4.7,5.4,2.));
#13310=CARTESIAN_POINT('',(4.7,5.4,10.));
#13311=CARTESIAN_POINT('Origin',(5.5,3.,10.));
#13312=CARTESIAN_POINT('Origin',(5.5,3.,2.));
#13313=CARTESIAN_POINT('',(0.,0.,0.));
#13314=CARTESIAN_POINT('Origin',(4.4,1.51507575950825,5.51507575950825));
#13315=CARTESIAN_POINT('',(4.5,1.51507575950825,5.74007575950825));
#13316=CARTESIAN_POINT('Origin',(4.5,1.51507575950825,5.51507575950825));
#13317=CARTESIAN_POINT('',(4.7,1.51507575950825,5.74007575950825));
#13318=CARTESIAN_POINT('',(4.4,1.51507575950825,5.74007575950825));
#13319=CARTESIAN_POINT('Origin',(4.7,1.51507575950825,5.51507575950825));
#13320=CARTESIAN_POINT('Origin',(4.4,1.51507575950825,8.48492424049175));
#13321=CARTESIAN_POINT('',(4.5,1.51507575950825,8.70992424049175));
#13322=CARTESIAN_POINT('Origin',(4.5,1.51507575950825,8.48492424049175));
#13323=CARTESIAN_POINT('',(4.7,1.51507575950825,8.70992424049175));
#13324=CARTESIAN_POINT('',(4.4,1.51507575950825,8.70992424049175));
#13325=CARTESIAN_POINT('Origin',(4.7,1.51507575950825,8.48492424049175));
#13326=CARTESIAN_POINT('Origin',(4.4,4.48492424049175,8.48492424049175));
#13327=CARTESIAN_POINT('',(4.5,4.48492424049175,8.70992424049175));
#13328=CARTESIAN_POINT('Origin',(4.5,4.48492424049175,8.48492424049175));
#13329=CARTESIAN_POINT('',(4.7,4.48492424049175,8.70992424049175));
#13330=CARTESIAN_POINT('',(4.4,4.48492424049175,8.70992424049175));
#13331=CARTESIAN_POINT('Origin',(4.7,4.48492424049175,8.48492424049175));
#13332=CARTESIAN_POINT('Origin',(4.4,4.48492424049175,5.51507575950825));
#13333=CARTESIAN_POINT('',(4.5,4.48492424049175,5.74007575950825));
#13334=CARTESIAN_POINT('Origin',(4.5,4.48492424049175,5.51507575950825));
#13335=CARTESIAN_POINT('',(4.7,4.48492424049175,5.74007575950825));
#13336=CARTESIAN_POINT('',(4.4,4.48492424049175,5.74007575950825));
#13337=CARTESIAN_POINT('Origin',(4.7,4.48492424049175,5.51507575950825));
#13338=CARTESIAN_POINT('Origin',(4.7,3.,7.));
#13339=CARTESIAN_POINT('',(5.,3.,8.59));
#13340=CARTESIAN_POINT('Origin',(5.,3.,7.));
#13341=CARTESIAN_POINT('',(4.7,3.,8.59));
#13342=CARTESIAN_POINT('',(4.7,3.,8.59));
#13343=CARTESIAN_POINT('Origin',(4.7,3.,7.));
#13344=CARTESIAN_POINT('Origin',(5.,3.,7.));
#13345=CARTESIAN_POINT('',(5.,3.,8.2));
#13346=CARTESIAN_POINT('Origin',(5.,3.,7.));
#13347=CARTESIAN_POINT('Origin',(4.5,3.,7.));
#13348=CARTESIAN_POINT('',(4.5,3.,8.2));
#13349=CARTESIAN_POINT('',(4.5,3.,8.2));
#13350=CARTESIAN_POINT('Origin',(4.5,3.,7.));
#13351=CARTESIAN_POINT('Origin',(4.5,3.,7.));
#13352=CARTESIAN_POINT('',(4.7,3.,9.4));
#13353=CARTESIAN_POINT('Origin',(4.7,3.,7.));
#13354=CARTESIAN_POINT('',(4.5,3.,9.4));
#13355=CARTESIAN_POINT('',(4.5,3.,9.4));
#13356=CARTESIAN_POINT('Origin',(4.5,3.,7.));
#13357=CARTESIAN_POINT('Origin',(4.7,3.,7.));
#13358=CARTESIAN_POINT('Origin',(4.5,3.,7.));
#13359=CARTESIAN_POINT('',(0.,0.,0.));
#13360=CARTESIAN_POINT('Origin',(6.2,1.51507575950825,5.51507575950825));
#13361=CARTESIAN_POINT('',(6.3,1.51507575950825,5.74007575950825));
#13362=CARTESIAN_POINT('Origin',(6.3,1.51507575950825,5.51507575950825));
#13363=CARTESIAN_POINT('',(6.5,1.51507575950825,5.74007575950825));
#13364=CARTESIAN_POINT('',(6.2,1.51507575950825,5.74007575950825));
#13365=CARTESIAN_POINT('Origin',(6.5,1.51507575950825,5.51507575950825));
#13366=CARTESIAN_POINT('Origin',(6.2,1.51507575950825,8.48492424049175));
#13367=CARTESIAN_POINT('',(6.3,1.51507575950825,8.70992424049175));
#13368=CARTESIAN_POINT('Origin',(6.3,1.51507575950825,8.48492424049175));
#13369=CARTESIAN_POINT('',(6.5,1.51507575950825,8.70992424049175));
#13370=CARTESIAN_POINT('',(6.2,1.51507575950825,8.70992424049175));
#13371=CARTESIAN_POINT('Origin',(6.5,1.51507575950825,8.48492424049175));
#13372=CARTESIAN_POINT('Origin',(6.2,4.48492424049175,8.48492424049175));
#13373=CARTESIAN_POINT('',(6.3,4.48492424049175,8.70992424049175));
#13374=CARTESIAN_POINT('Origin',(6.3,4.48492424049175,8.48492424049175));
#13375=CARTESIAN_POINT('',(6.5,4.48492424049175,8.70992424049175));
#13376=CARTESIAN_POINT('',(6.2,4.48492424049175,8.70992424049175));
#13377=CARTESIAN_POINT('Origin',(6.5,4.48492424049175,8.48492424049175));
#13378=CARTESIAN_POINT('Origin',(6.2,4.48492424049175,5.51507575950825));
#13379=CARTESIAN_POINT('',(6.3,4.48492424049175,5.74007575950825));
#13380=CARTESIAN_POINT('Origin',(6.3,4.48492424049175,5.51507575950825));
#13381=CARTESIAN_POINT('',(6.5,4.48492424049175,5.74007575950825));
#13382=CARTESIAN_POINT('',(6.2,4.48492424049175,5.74007575950825));
#13383=CARTESIAN_POINT('Origin',(6.5,4.48492424049175,5.51507575950825));
#13384=CARTESIAN_POINT('Origin',(6.,3.,7.));
#13385=CARTESIAN_POINT('',(6.3,3.,8.59));
#13386=CARTESIAN_POINT('Origin',(6.3,3.,7.));
#13387=CARTESIAN_POINT('',(6.,3.,8.59));
#13388=CARTESIAN_POINT('',(6.,3.,8.59));
#13389=CARTESIAN_POINT('Origin',(6.,3.,7.));
#13390=CARTESIAN_POINT('Origin',(6.,3.,7.));
#13391=CARTESIAN_POINT('',(6.,3.,8.2));
#13392=CARTESIAN_POINT('Origin',(6.,3.,7.));
#13393=CARTESIAN_POINT('Origin',(6.3,3.,7.));
#13394=CARTESIAN_POINT('',(6.5,3.,8.2));
#13395=CARTESIAN_POINT('Origin',(6.5,3.,7.));
#13396=CARTESIAN_POINT('',(6.3,3.,8.2));
#13397=CARTESIAN_POINT('Origin',(6.3,3.,7.));
#13398=CARTESIAN_POINT('',(6.5,3.,9.4));
#13399=CARTESIAN_POINT('Origin',(6.5,3.,7.));
#13400=CARTESIAN_POINT('',(6.3,3.,9.4));
#13401=CARTESIAN_POINT('',(6.3,3.,9.4));
#13402=CARTESIAN_POINT('Origin',(6.3,3.,7.));
#13403=CARTESIAN_POINT('Origin',(6.5,3.,7.));
#13404=CARTESIAN_POINT('Origin',(6.3,3.,7.));
#13405=CARTESIAN_POINT('',(0.,0.,0.));
#13406=CARTESIAN_POINT('Origin',(5.5,7.9,4.));
#13407=CARTESIAN_POINT('',(5.25,8.,4.));
#13408=CARTESIAN_POINT('Origin',(5.5,8.,4.));
#13409=CARTESIAN_POINT('',(5.25,9.,4.));
#13410=CARTESIAN_POINT('',(5.25,7.9,4.));
#13411=CARTESIAN_POINT('Origin',(5.5,9.,4.));
#13412=CARTESIAN_POINT('Origin',(-0.3,7.9,4.));
#13413=CARTESIAN_POINT('',(-0.55,8.,4.));
#13414=CARTESIAN_POINT('Origin',(-0.3,8.,4.));
#13415=CARTESIAN_POINT('',(-0.55,9.,4.));
#13416=CARTESIAN_POINT('',(-0.55,7.9,4.));
#13417=CARTESIAN_POINT('Origin',(-0.3,9.,4.));
#13418=CARTESIAN_POINT('Origin',(7.,8.5,1.6));
#13419=CARTESIAN_POINT('',(6.6,8.5,1.6));
#13420=CARTESIAN_POINT('Origin',(7.,8.5,1.6));
#13421=CARTESIAN_POINT('',(6.6,8.5,6.));
#13422=CARTESIAN_POINT('',(6.6,8.5,1.6));
#13423=CARTESIAN_POINT('Origin',(7.,8.5,6.));
#13424=CARTESIAN_POINT('Origin',(7.,8.5,1.6));
#13425=CARTESIAN_POINT('',(6.775,8.5,1.6));
#13426=CARTESIAN_POINT('Origin',(7.,8.5,1.6));
#13427=CARTESIAN_POINT('Origin',(7.,8.5,0.9));
#13428=CARTESIAN_POINT('',(6.775,8.5,1.));
#13429=CARTESIAN_POINT('Origin',(7.,8.5,1.));
#13430=CARTESIAN_POINT('',(6.775,8.5,0.9));
#13431=CARTESIAN_POINT('Origin',(-1.5,8.5,1.6));
#13432=CARTESIAN_POINT('',(-1.9,8.5,1.6));
#13433=CARTESIAN_POINT('Origin',(-1.5,8.5,1.6));
#13434=CARTESIAN_POINT('',(-1.9,8.5,6.));
#13435=CARTESIAN_POINT('',(-1.9,8.5,1.6));
#13436=CARTESIAN_POINT('Origin',(-1.5,8.5,6.));
#13437=CARTESIAN_POINT('Origin',(-1.5,8.5,1.6));
#13438=CARTESIAN_POINT('',(-1.725,8.5,1.6));
#13439=CARTESIAN_POINT('Origin',(-1.5,8.5,1.6));
#13440=CARTESIAN_POINT('Origin',(-1.5,8.5,0.9));
#13441=CARTESIAN_POINT('',(-1.725,8.5,1.));
#13442=CARTESIAN_POINT('Origin',(-1.5,8.5,1.));
#13443=CARTESIAN_POINT('',(-1.725,8.5,0.9));
#13444=CARTESIAN_POINT('Origin',(8.,9.,1.));
#13445=CARTESIAN_POINT('',(8.,9.,1.));
#13446=CARTESIAN_POINT('',(-2.5,9.,1.));
#13447=CARTESIAN_POINT('',(8.,9.,1.));
#13448=CARTESIAN_POINT('',(-2.5,9.,6.));
#13449=CARTESIAN_POINT('',(-2.5,9.,1.));
#13450=CARTESIAN_POINT('',(8.,9.,6.));
#13451=CARTESIAN_POINT('',(8.,9.,6.));
#13452=CARTESIAN_POINT('',(8.,9.,1.));
#13453=CARTESIAN_POINT('Origin',(8.,8.,1.));
#13454=CARTESIAN_POINT('',(8.,8.,1.));
#13455=CARTESIAN_POINT('',(8.,8.,1.));
#13456=CARTESIAN_POINT('',(8.,8.,6.));
#13457=CARTESIAN_POINT('',(8.,8.,6.));
#13458=CARTESIAN_POINT('',(8.,8.,1.));
#13459=CARTESIAN_POINT('Origin',(-2.5,8.,1.));
#13460=CARTESIAN_POINT('',(-2.5,8.,1.));
#13461=CARTESIAN_POINT('',(-2.5,8.,1.));
#13462=CARTESIAN_POINT('',(-2.5,8.,6.));
#13463=CARTESIAN_POINT('',(-2.5,8.,6.));
#13464=CARTESIAN_POINT('',(-2.5,8.,1.));
#13465=CARTESIAN_POINT('Origin',(-2.5,9.,1.));
#13466=CARTESIAN_POINT('',(-2.5,9.,1.));
#13467=CARTESIAN_POINT('',(-2.5,9.,6.));
#13468=CARTESIAN_POINT('Origin',(2.75,8.5,6.));
#13469=CARTESIAN_POINT('Origin',(2.75,8.5,1.));
#13470=CARTESIAN_POINT('',(0.,0.,0.));
#13471=CARTESIAN_POINT('Origin',(-0.3,5.4,4.));
#13472=CARTESIAN_POINT('',(-1.,5.7,4.));
#13473=CARTESIAN_POINT('Origin',(-0.3,5.7,4.));
#13474=CARTESIAN_POINT('',(-1.,5.4,4.));
#13475=CARTESIAN_POINT('',(-1.,5.4,4.));
#13476=CARTESIAN_POINT('Origin',(-0.3,5.4,4.));
#13477=CARTESIAN_POINT('Origin',(-0.3,5.7,4.));
#13478=CARTESIAN_POINT('Origin',(-0.3,5.4,4.));
#13479=CARTESIAN_POINT('',(0.,0.,0.));
#13480=CARTESIAN_POINT('Origin',(-0.3,7.1,4.));
#13481=CARTESIAN_POINT('',(-1.,7.4,4.));
#13482=CARTESIAN_POINT('Origin',(-0.3,7.4,4.));
#13483=CARTESIAN_POINT('',(-1.,7.1,4.));
#13484=CARTESIAN_POINT('',(-1.,7.1,4.));
#13485=CARTESIAN_POINT('Origin',(-0.3,7.1,4.));
#13486=CARTESIAN_POINT('Origin',(-0.3,7.4,4.));
#13487=CARTESIAN_POINT('Origin',(-0.3,7.1,4.));
#13488=CARTESIAN_POINT('',(0.,0.,0.));
#13489=CARTESIAN_POINT('Ctrl Pts',(0.0999994223174587,7.09981632447119,
4.00428180053801));
#13490=CARTESIAN_POINT('Ctrl Pts',(0.0999933436797077,7.09594376396835,
4.04933684813297));
#13491=CARTESIAN_POINT('Ctrl Pts',(0.0846594327171957,7.08819408394972,
4.13908992957458));
#13492=CARTESIAN_POINT('Ctrl Pts',(-0.00357043069494361,7.07263318914228,
4.29963340285418));
#13493=CARTESIAN_POINT('Ctrl Pts',(-0.206356294917572,7.05308143195573,
4.42766373470968));
#13494=CARTESIAN_POINT('Ctrl Pts',(-0.494863120131574,7.02945164505109,
4.39548903188326));
#13495=CARTESIAN_POINT('Ctrl Pts',(-0.701612481834811,7.00565862484048,
4.18915927264886));
#13496=CARTESIAN_POINT('Ctrl Pts',(-0.734902354617378,6.98170298771966,
3.89687986754614));
#13497=CARTESIAN_POINT('Ctrl Pts',(-0.577665286755769,6.9575878275568,3.64601239877861));
#13498=CARTESIAN_POINT('Ctrl Pts',(-0.296425446296891,6.93331589731144,
3.54721069783272));
#13499=CARTESIAN_POINT('Ctrl Pts',(-0.0238970429973844,6.90979548741706,
3.64245102870328));
#13500=CARTESIAN_POINT('Ctrl Pts',(0.131586191166419,6.88704931445005,3.8704985271515));
#13501=CARTESIAN_POINT('Ctrl Pts',(0.132036205657411,6.86509836852865,4.13674945418924));
#13502=CARTESIAN_POINT('Ctrl Pts',(-0.0060413687179679,6.84487478558125,
4.33958298894643));
#13503=CARTESIAN_POINT('Ctrl Pts',(-0.204116844890033,6.82641141958407,
4.43475944317313));
#13504=CARTESIAN_POINT('Ctrl Pts',(-0.402473369433673,6.80973569344043,
4.43486896119673));
#13505=CARTESIAN_POINT('Ctrl Pts',(-0.581827228221285,6.79300305116116,
4.34852221416367));
#13506=CARTESIAN_POINT('Ctrl Pts',(-0.706454134874152,6.7762153628094,4.192464816352));
#13507=CARTESIAN_POINT('Ctrl Pts',(-0.751016294559626,6.75937457420164,
3.99715087739011));
#13508=CARTESIAN_POINT('Ctrl Pts',(-0.706447662037028,6.74248271608976,
3.80123388795173));
#13509=CARTESIAN_POINT('Ctrl Pts',(-0.580873534358325,6.72554188917784,
3.64359934962882));
#13510=CARTESIAN_POINT('Ctrl Pts',(-0.398793807750649,6.70855427056295,
3.55588854173989));
#13511=CARTESIAN_POINT('Ctrl Pts',(-0.196213186746174,6.69152210478501,
3.55582569363604));
#13512=CARTESIAN_POINT('Ctrl Pts',(-0.0130963934752721,6.67444770586136,
3.64392728654252));
#13513=CARTESIAN_POINT('Ctrl Pts',(0.113707820363769,6.65733344528682,3.80305624025719));
#13514=CARTESIAN_POINT('Ctrl Pts',(0.164656362590817,6.63827601697293,4.02413741573514));
#13515=CARTESIAN_POINT('Ctrl Pts',(0.0896082709820025,6.61726302509207,
4.2676978223342));
#13516=CARTESIAN_POINT('Ctrl Pts',(-0.110245732077343,6.59619863179822,
4.4270642600818));
#13517=CARTESIAN_POINT('Ctrl Pts',(-0.290838098938005,6.58084997747224,
4.45395573001046));
#13518=CARTESIAN_POINT('Ctrl Pts',(-0.445467117475853,6.56740673782488,
4.43069910759464));
#13519=CARTESIAN_POINT('Ctrl Pts',(-0.589663880409842,6.55395079532829,
4.36131796304211));
#13520=CARTESIAN_POINT('Ctrl Pts',(-0.718225707768932,6.53662851071928,
4.20020661739991));
#13521=CARTESIAN_POINT('Ctrl Pts',(-0.763898158866166,6.51928717897976,
3.99912848715837));
#13522=CARTESIAN_POINT('Ctrl Pts',(-0.710721419612997,6.49903664059857,
3.764202830041));
#13523=CARTESIAN_POINT('Ctrl Pts',(-0.510149997687367,6.47587070043553,
3.56253207697483));
#13524=CARTESIAN_POINT('Ctrl Pts',(-0.227250362890276,6.45268625633124,
3.53107252428385));
#13525=CARTESIAN_POINT('Ctrl Pts',(-0.00982453983942397,6.43239259089565,
3.63631313688574));
#13526=CARTESIAN_POINT('Ctrl Pts',(0.119224416062016,6.414995879623,3.79796488057796));
#13527=CARTESIAN_POINT('Ctrl Pts',(0.161414220224748,6.39904954972701,3.98302626625864));
#13528=CARTESIAN_POINT('Ctrl Pts',(0.132781651753175,6.38455548538367,4.15109736344141));
#13529=CARTESIAN_POINT('Ctrl Pts',(0.058591217696994,6.37151403493753,4.28547086198332));
#13530=CARTESIAN_POINT('Ctrl Pts',(-0.0558362639783319,6.35847699034469,
4.38747481451575));
#13531=CARTESIAN_POINT('Ctrl Pts',(-0.244624220570673,6.34110173177432,
4.46620946091905));
#13532=CARTESIAN_POINT('Ctrl Pts',(-0.509258386493358,6.31939963958705,
4.43663450707748));
#13533=CARTESIAN_POINT('Ctrl Pts',(-0.735030443095589,6.29339375292805,
4.21063569075453));
#13534=CARTESIAN_POINT('Ctrl Pts',(-0.770492148406669,6.2674338232997,3.89395438143295));
#13535=CARTESIAN_POINT('Ctrl Pts',(-0.601210048531917,6.24152902186401,
3.62457992816658));
#13536=CARTESIAN_POINT('Ctrl Pts',(-0.351688619951789,6.21999512440529,
3.53770552245775));
#13537=CARTESIAN_POINT('Ctrl Pts',(-0.152299417857812,6.20280445728418,
3.57207084012085));
#13538=CARTESIAN_POINT('Ctrl Pts',(-0.00495835013055459,6.18850033974624,
3.65330634586973));
#13539=CARTESIAN_POINT('Ctrl Pts',(0.111522803781729,6.17279483671223,3.79940640678234));
#13540=CARTESIAN_POINT('Ctrl Pts',(0.156701474788417,6.15570021231953,3.99770463755195));
#13541=CARTESIAN_POINT('Ctrl Pts',(0.115262604711903,6.14006777305336,4.17897821875209));
#13542=CARTESIAN_POINT('Ctrl Pts',(0.0185932180471106,6.12588811043834,
4.31497113433199));
#13543=CARTESIAN_POINT('Ctrl Pts',(-0.103590553659916,6.11315178814851,
4.4016989608744));
#13544=CARTESIAN_POINT('Ctrl Pts',(-0.247293954733903,6.1004417858412,4.44304193852122));
#13545=CARTESIAN_POINT('Ctrl Pts',(-0.412869049658234,6.08634982725544,
4.43379507168706));
#13546=CARTESIAN_POINT('Ctrl Pts',(-0.578482300908516,6.07088880084204,
4.3539190346138));
#13547=CARTESIAN_POINT('Ctrl Pts',(-0.703246723757797,6.05407432044984,
4.19753682982269));
#13548=CARTESIAN_POINT('Ctrl Pts',(-0.747469580607062,6.03731392465469,
4.00314057125818));
#13549=CARTESIAN_POINT('Ctrl Pts',(-0.703238625925696,6.02060951959296,
3.80940575329504));
#13550=CARTESIAN_POINT('Ctrl Pts',(-0.579634776479789,6.00396293095479,
3.65467865258803));
#13551=CARTESIAN_POINT('Ctrl Pts',(-0.431500759601328,5.99014040360805,
3.58338254073736));
#13552=CARTESIAN_POINT('Ctrl Pts',(-0.303561319206374,5.97911298339926,
3.56906449106088));
#13553=CARTESIAN_POINT('Ctrl Pts',(-0.207808748835976,5.97085791464426,
3.57983145987356));
#13554=CARTESIAN_POINT('Ctrl Pts',(-0.117044922248722,5.96261853714979,
3.6116348383249));
#13555=CARTESIAN_POINT('Ctrl Pts',(-0.00861997369778145,5.95165386736835,
3.67968231581426));
#13556=CARTESIAN_POINT('Ctrl Pts',(0.0926329081004657,5.93798817658918,
3.80681756846826));
#13557=CARTESIAN_POINT('Ctrl Pts',(0.135870644163702,5.92165495155963,3.99626375633351));
#13558=CARTESIAN_POINT('Ctrl Pts',(0.0926387969430078,5.90538860209907,
4.18487776410349));
#13559=CARTESIAN_POINT('Ctrl Pts',(-0.0175125738479973,5.89054016294629,
4.32293582509909));
#13560=CARTESIAN_POINT('Ctrl Pts',(-0.156061008534171,5.87709197920747,
4.39936287338782));
#13561=CARTESIAN_POINT('Ctrl Pts',(-0.296018497756522,5.86502791432804,
4.42315611503599));
#13562=CARTESIAN_POINT('Ctrl Pts',(-0.435406476921251,5.8530035361086,4.39932451423293));
#13563=CARTESIAN_POINT('Ctrl Pts',(-0.600212844195293,5.83702437044493,
4.30861645270809));
#13564=CARTESIAN_POINT('Ctrl Pts',(-0.729945333339283,5.81715142573852,
4.10216892170714));
#13565=CARTESIAN_POINT('Ctrl Pts',(-0.696976009348358,5.7934671926544,3.81306008549607));
#13566=CARTESIAN_POINT('Ctrl Pts',(-0.492652698548329,5.76994854996481,
3.60918617550531));
#13567=CARTESIAN_POINT('Ctrl Pts',(-0.207515825799976,5.74659510021081,
3.57736699868709));
#13568=CARTESIAN_POINT('Ctrl Pts',(-0.00714719245692835,5.72727465695078,
3.70390131122158));
#13569=CARTESIAN_POINT('Ctrl Pts',(0.0800330609517386,5.71189866882786,
3.86253474741929));
#13570=CARTESIAN_POINT('Ctrl Pts',(0.0951821641861108,5.70424160396714,
3.95121652410011));
#13571=CARTESIAN_POINT('Ctrl Pts',(0.0951881709252366,5.70041484319491,
3.99573871784903));
#13572=CARTESIAN_POINT('Ctrl Pts',(0.0850394574365172,7.09981632447119,
4.00427978220239));
#13573=CARTESIAN_POINT('Ctrl Pts',(0.0850336018816217,7.09608588493208,
4.04768133289773));
#13574=CARTESIAN_POINT('Ctrl Pts',(0.0702699903358584,7.08862397630483,
4.1341064684711));
#13575=CARTESIAN_POINT('Ctrl Pts',(-0.0147069746650678,7.07363615104764,
4.28874312195255));
#13576=CARTESIAN_POINT('Ctrl Pts',(-0.210062520100004,7.05480250014203,
4.4121050616425));
#13577=CARTESIAN_POINT('Ctrl Pts',(-0.488174822436898,7.03202630176359,
4.38112095270672));
#13578=CARTESIAN_POINT('Ctrl Pts',(-0.687626117343361,7.0090788623615,4.18212006759028));
#13579=CARTESIAN_POINT('Ctrl Pts',(-0.719801750366849,6.98595686154072,
3.89998017636458));
#13580=CARTESIAN_POINT('Ctrl Pts',(-0.567925280966783,6.9626613445872,3.65757702153162));
#13581=CARTESIAN_POINT('Ctrl Pts',(-0.295960145703228,6.93919201998295,
3.56197635348132));
#13582=CARTESIAN_POINT('Ctrl Pts',(-0.0321049966673812,6.91642613922016,
3.65412444008679));
#13583=CARTESIAN_POINT('Ctrl Pts',(0.118620874938022,6.89438553806723,3.87511047955543));
#13584=CARTESIAN_POINT('Ctrl Pts',(0.119105685200114,6.87309055560467,4.13343111127147));
#13585=CARTESIAN_POINT('Ctrl Pts',(-0.0149725090072682,6.85345021204612,
4.33047273617547));
#13586=CARTESIAN_POINT('Ctrl Pts',(-0.207553265723982,6.83550152476108,
4.42303755552263));
#13587=CARTESIAN_POINT('Ctrl Pts',(-0.400605820874248,6.81927426099695,
4.42316739110795));
#13588=CARTESIAN_POINT('Ctrl Pts',(-0.575349585461221,6.80297292453282,
4.3390616393177));
#13589=CARTESIAN_POINT('Ctrl Pts',(-0.696901935083712,6.78660524474866,
4.18689685110264));
#13590=CARTESIAN_POINT('Ctrl Pts',(-0.740422898887374,6.77016837055957,
3.99624089239393));
#13591=CARTESIAN_POINT('Ctrl Pts',(-0.696895127946879,6.75366348159961,
3.80478155122518));
#13592=CARTESIAN_POINT('Ctrl Pts',(-0.57406933450842,6.73709380592631,3.65055798081225));
#13593=CARTESIAN_POINT('Ctrl Pts',(-0.395769076508023,6.72046256251377,
3.56463827820055));
#13594=CARTESIAN_POINT('Ctrl Pts',(-0.197154892631745,6.70376777233271,
3.56455003028145));
#13595=CARTESIAN_POINT('Ctrl Pts',(-0.0174072167564555,6.68701354119935,
3.65099852210416));
#13596=CARTESIAN_POINT('Ctrl Pts',(0.107219695584159,6.67019963849409,3.80735503098315));
#13597=CARTESIAN_POINT('Ctrl Pts',(0.157377024534706,6.65145770741293,4.02484224001632));
#13598=CARTESIAN_POINT('Ctrl Pts',(0.0834907936109698,6.63075558432489,
4.26482879249461));
#13599=CARTESIAN_POINT('Ctrl Pts',(-0.113676877997255,6.60997502326179,
4.4221382080455));
#13600=CARTESIAN_POINT('Ctrl Pts',(-0.292136244859537,6.5948103064137,4.44873719553528));
#13601=CARTESIAN_POINT('Ctrl Pts',(-0.445072347899979,6.58151560551988,
4.42573828157157));
#13602=CARTESIAN_POINT('Ctrl Pts',(-0.587808705388691,6.56819972291512,
4.35708244751097));
#13603=CARTESIAN_POINT('Ctrl Pts',(-0.715254356693917,6.55103194356631,
4.19742039979326));
#13604=CARTESIAN_POINT('Ctrl Pts',(-0.760601355295959,6.53382909817788,
3.99789591592248));
#13605=CARTESIAN_POINT('Ctrl Pts',(-0.7078026422373,6.51371065102388,3.76447139208622));
#13606=CARTESIAN_POINT('Ctrl Pts',(-0.508287882172965,6.49066883804046,
3.56373316987723));
#13607=CARTESIAN_POINT('Ctrl Pts',(-0.226234240731051,6.46755740591608,
3.53227686762576));
#13608=CARTESIAN_POINT('Ctrl Pts',(-0.00909244890320504,6.44729795655168,
3.63734053951694));
#13609=CARTESIAN_POINT('Ctrl Pts',(0.119970850340226,6.42990267527582,3.79896825205898));
#13610=CARTESIAN_POINT('Ctrl Pts',(0.162236447406711,6.41394240449883,3.98423317997473));
#13611=CARTESIAN_POINT('Ctrl Pts',(0.133549532561585,6.39941634657213,4.15269512343536));
#13612=CARTESIAN_POINT('Ctrl Pts',(0.059128979758546,6.38633399253393,4.28751171624146));
#13613=CARTESIAN_POINT('Ctrl Pts',(-0.0557735754439485,6.37324413074094,
4.38995105707331));
#13614=CARTESIAN_POINT('Ctrl Pts',(-0.245522966737918,6.35578135522631,
4.46910560844112));
#13615=CARTESIAN_POINT('Ctrl Pts',(-0.511891841221142,6.33394317857852,
4.43941437761895));
#13616=CARTESIAN_POINT('Ctrl Pts',(-0.73964230083353,6.30772004879476,4.21157475252753));
#13617=CARTESIAN_POINT('Ctrl Pts',(-0.775562357309942,6.28150419722604,
3.89165585318146));
#13618=CARTESIAN_POINT('Ctrl Pts',(-0.604311957412975,6.25529235214756,
3.61896952975546));
#13619=CARTESIAN_POINT('Ctrl Pts',(-0.351351084360445,6.23346807877194,
3.53081646027971));
#13620=CARTESIAN_POINT('Ctrl Pts',(-0.148911855072523,6.21601731725428,
3.56569131592939));
#13621=CARTESIAN_POINT('Ctrl Pts',(0.000808738546099167,6.20148503609852,
3.64822598806359));
#13622=CARTESIAN_POINT('Ctrl Pts',(0.119307888319452,6.18551200572715,3.79681481925343));
#13623=CARTESIAN_POINT('Ctrl Pts',(0.165336825909723,6.16810621199183,3.99873450926149));
#13624=CARTESIAN_POINT('Ctrl Pts',(0.12311936738889,6.15217178129263,4.1835309684545));
#13625=CARTESIAN_POINT('Ctrl Pts',(0.024491947298141,6.13770537799267,4.32229762424903));
#13626=CARTESIAN_POINT('Ctrl Pts',(-0.10026800379765,6.12470150020605,4.41086793897621));
#13627=CARTESIAN_POINT('Ctrl Pts',(-0.247118546887194,6.1117152886378,4.45312483699181));
#13628=CARTESIAN_POINT('Ctrl Pts',(-0.416459720890053,6.09730438243501,
4.44367875235149));
#13629=CARTESIAN_POINT('Ctrl Pts',(-0.585994266630716,6.08147960761965,
4.36192882635867));
#13630=CARTESIAN_POINT('Ctrl Pts',(-0.71384850238361,6.06425381154321,4.20171116423524));
#13631=CARTESIAN_POINT('Ctrl Pts',(-0.759222000808869,6.04706459967159,
4.00233367493855));
#13632=CARTESIAN_POINT('Ctrl Pts',(-0.713838394267311,6.02991914561157,
3.80345284952215));
#13633=CARTESIAN_POINT('Ctrl Pts',(-0.58685029737105,6.01281745749491,3.64446602567488));
#13634=CARTESIAN_POINT('Ctrl Pts',(-0.434523741076119,5.99860459894777,
3.57113647661554));
#13635=CARTESIAN_POINT('Ctrl Pts',(-0.302871593009492,5.98725781105221,
3.55640154880377));
#13636=CARTESIAN_POINT('Ctrl Pts',(-0.204299994389332,5.97875983751493,
3.56748322724138));
#13637=CARTESIAN_POINT('Ctrl Pts',(-0.110827457753729,5.97027500248914,
3.60023416597451));
#13638=CARTESIAN_POINT('Ctrl Pts',(0.000877339158924813,5.95897911565719,
3.67033627955141));
#13639=CARTESIAN_POINT('Ctrl Pts',(0.105257286966471,5.94489365179489,3.80137990843985));
#13640=CARTESIAN_POINT('Ctrl Pts',(0.149873797036135,5.92804610367806,3.99679794750918));
#13641=CARTESIAN_POINT('Ctrl Pts',(0.105257359738255,5.91125630747322,4.19149770579706));
#13642=CARTESIAN_POINT('Ctrl Pts',(-0.00851130012522223,5.89591960107197,
4.33410736914532));
#13643=CARTESIAN_POINT('Ctrl Pts',(-0.151696220437804,5.88202155769958,
4.41309722089718));
#13644=CARTESIAN_POINT('Ctrl Pts',(-0.296398986774869,5.86954879341379,
4.43770080209349));
#13645=CARTESIAN_POINT('Ctrl Pts',(-0.440573237144837,5.85711192694754,
4.41305386836028));
#13646=CARTESIAN_POINT('Ctrl Pts',(-0.611104421885485,5.84057809075553,
4.31920084666369));
#13647=CARTESIAN_POINT('Ctrl Pts',(-0.745431119265092,5.82000461576502,
4.10548372373842));
#13648=CARTESIAN_POINT('Ctrl Pts',(-0.711300999956552,5.79546993853416,
3.80598914689769));
#13649=CARTESIAN_POINT('Ctrl Pts',(-0.499541348546689,5.77109407410407,
3.59467599283417));
#13650=CARTESIAN_POINT('Ctrl Pts',(-0.203895328638292,5.7468798977641,3.56167095656836));
#13651=CARTESIAN_POINT('Ctrl Pts',(0.00392749184947024,5.72684068907964,
3.6929091997083));
#13652=CARTESIAN_POINT('Ctrl Pts',(0.0943564738679285,5.7108922189658,3.85744827453292));
#13653=CARTESIAN_POINT('Ctrl Pts',(0.110072470175732,5.70294882509164,3.94944546934011));
#13654=CARTESIAN_POINT('Ctrl Pts',(0.110078698955025,5.69898060743533,3.99561343380099));
#13655=CARTESIAN_POINT('Ctrl Pts',(0.0552109446983192,7.08554097311938,
4.00304876633418));
#13656=CARTESIAN_POINT('Ctrl Pts',(0.0552055358490416,7.08209511947001,
4.04313932142398));
#13657=CARTESIAN_POINT('Ctrl Pts',(0.0415778810591391,7.07520994153035,
4.12288334405912));
#13658=CARTESIAN_POINT('Ctrl Pts',(-0.0367895863384045,7.06138952221764,
4.26547075358216));
#13659=CARTESIAN_POINT('Ctrl Pts',(-0.216751774778633,7.04404262129843,
4.37904913409819));
#13660=CARTESIAN_POINT('Ctrl Pts',(-0.472633848843551,7.0230861784788,4.35049327462187));
#13661=CARTESIAN_POINT('Ctrl Pts',(-0.655980880788529,7.00198852558813,
4.16750943496815));
#13662=CARTESIAN_POINT('Ctrl Pts',(-0.685529083724197,6.98073994105562,
3.90823429417137));
#13663=CARTESIAN_POINT('Ctrl Pts',(-0.545981564425269,6.95933520737526,
3.68551901603162));
#13664=CARTESIAN_POINT('Ctrl Pts',(-0.296075489511932,6.93776772965475,
3.59766361550569));
#13665=CARTESIAN_POINT('Ctrl Pts',(-0.0535123959286835,6.91683750495745,
3.68235541997892));
#13666=CARTESIAN_POINT('Ctrl Pts',(0.0851561523655047,6.89656078808882,
3.88562267842967));
#13667=CARTESIAN_POINT('Ctrl Pts',(0.0856311510431353,6.87695461538451,
4.12343923801433));
#13668=CARTESIAN_POINT('Ctrl Pts',(-0.037907049429957,6.85885216444035,
4.30504970436046));
#13669=CARTESIAN_POINT('Ctrl Pts',(-0.215577868848402,6.84229013135253,
4.3904699811323));
#13670=CARTESIAN_POINT('Ctrl Pts',(-0.393871042935876,6.82730164024858,
4.39060863287945));
#13671=CARTESIAN_POINT('Ctrl Pts',(-0.555445579066094,6.81222960735315,
4.31286947512227));
#13672=CARTESIAN_POINT('Ctrl Pts',(-0.667991397971185,6.7970745501898,4.17201470408707));
#13673=CARTESIAN_POINT('Ctrl Pts',(-0.708363930243454,6.78183538373591,
3.99528088580219));
#13674=CARTESIAN_POINT('Ctrl Pts',(-0.667982499492249,6.76651159301788,
3.8175383544735));
#13675=CARTESIAN_POINT('Ctrl Pts',(-0.553809065445986,6.75110329506063,
3.67412832553629));
#13676=CARTESIAN_POINT('Ctrl Pts',(-0.387770718002321,6.73561041405154,
3.59408217536656));
#13677=CARTESIAN_POINT('Ctrl Pts',(-0.202486939836806,6.72003270044929,
3.59396650356072));
#13678=CARTESIAN_POINT('Ctrl Pts',(-0.0344849723331165,6.70437042642184,
3.67472585533919));
#13679=CARTESIAN_POINT('Ctrl Pts',(0.0822359686491668,6.6886238248135,3.82110359305832));
#13680=CARTESIAN_POINT('Ctrl Pts',(0.129333318074877,6.6710343619389,4.02513087435611));
#13681=CARTESIAN_POINT('Ctrl Pts',(0.0599513621413444,6.65156705091096,
4.25082146699634));
#13682=CARTESIAN_POINT('Ctrl Pts',(-0.125925468004263,6.63196518614269,
4.39924834947929));
#13683=CARTESIAN_POINT('Ctrl Pts',(-0.294649097744615,6.61762494437181,
4.42443992623928));
#13684=CARTESIAN_POINT('Ctrl Pts',(-0.439454924581737,6.60503562813921,
4.40266660815905));
#13685=CARTESIAN_POINT('Ctrl Pts',(-0.574832950582178,6.59240466995411,
4.33759318223502));
#13686=CARTESIAN_POINT('Ctrl Pts',(-0.696005607230916,6.57608629127481,
4.1858707309457));
#13687=CARTESIAN_POINT('Ctrl Pts',(-0.739264156798592,6.55968976182242,
3.99576554731973));
#13688=CARTESIAN_POINT('Ctrl Pts',(-0.688894544701315,6.54047191876598,
3.77281394895871));
#13689=CARTESIAN_POINT('Ctrl Pts',(-0.497850728795945,6.51838274700366,
3.58035881577739));
#13690=CARTESIAN_POINT('Ctrl Pts',(-0.226591456204558,6.49614979205781,
3.54992745923014));
#13691=CARTESIAN_POINT('Ctrl Pts',(-0.0170228957665506,6.47659384394549,
3.65124693095961));
#13692=CARTESIAN_POINT('Ctrl Pts',(0.107878534876526,6.45976489129137,3.80756740153316));
#13693=CARTESIAN_POINT('Ctrl Pts',(0.148935258357734,6.44427701128731,3.98728011631239));
#13694=CARTESIAN_POINT('Ctrl Pts',(0.121070920781021,6.43015138549249,4.15108396416147));
#13695=CARTESIAN_POINT('Ctrl Pts',(0.0485868461854486,6.41740335767032,
4.28244796483226));
#13696=CARTESIAN_POINT('Ctrl Pts',(-0.0635788152688685,6.40462128856916,
4.38248248865166));
#13697=CARTESIAN_POINT('Ctrl Pts',(-0.249190470547445,6.38753474317254,
4.45995182159303));
#13698=CARTESIAN_POINT('Ctrl Pts',(-0.510621805419283,6.36609553105664,
4.43099932549576));
#13699=CARTESIAN_POINT('Ctrl Pts',(-0.735220544630679,6.3402506864649,4.20663986268119));
#13700=CARTESIAN_POINT('Ctrl Pts',(-0.770998171812698,6.31429203879871,
3.89005168056026));
#13701=CARTESIAN_POINT('Ctrl Pts',(-0.601002821637636,6.28823331590632,
3.61892894068927));
#13702=CARTESIAN_POINT('Ctrl Pts',(-0.348588870206163,6.26643951526414,
3.53076923929659));
#13703=CARTESIAN_POINT('Ctrl Pts',(-0.145904386441107,6.24896558866351,
3.56564777464724));
#13704=CARTESIAN_POINT('Ctrl Pts',(0.00431784369931261,6.23438222817505,
3.64842497686876));
#13705=CARTESIAN_POINT('Ctrl Pts',(0.123537769777284,6.21831525558541,3.79782624277368));
#13706=CARTESIAN_POINT('Ctrl Pts',(0.170025222345384,6.20075900678011,4.0014515149975));
#13707=CARTESIAN_POINT('Ctrl Pts',(0.127382100777052,6.18464189141261,4.18835406447036));
#13708=CARTESIAN_POINT('Ctrl Pts',(0.0274168012845219,6.16997297685647,
4.32905626517445));
#13709=CARTESIAN_POINT('Ctrl Pts',(-0.0993153752368822,6.15675918917126,
4.41905554753229));
#13710=CARTESIAN_POINT('Ctrl Pts',(-0.248808689491018,6.14353471820731,
4.46210209715592));
#13711=CARTESIAN_POINT('Ctrl Pts',(-0.421546420510728,6.12883206416157,
4.45249609505736));
#13712=CARTESIAN_POINT('Ctrl Pts',(-0.594922024953856,6.11264861980656,
4.36896482777448));
#13713=CARTESIAN_POINT('Ctrl Pts',(-0.726050316003777,6.09498288711894,
4.20473974459702));
#13714=CARTESIAN_POINT('Ctrl Pts',(-0.772757113366257,6.07731254500321,
3.99981370250454));
#13715=CARTESIAN_POINT('Ctrl Pts',(-0.726037252404702,6.05963671350822,
3.79481962943994));
#13716=CARTESIAN_POINT('Ctrl Pts',(-0.594870280365665,6.04196116089001,
3.63048998551027));
#13717=CARTESIAN_POINT('Ctrl Pts',(-0.437085933471611,6.02723405694994,
3.55447714399662));
#13718=CARTESIAN_POINT('Ctrl Pts',(-0.300449841085889,6.01545653985552,
3.53917140938389));
#13719=CARTESIAN_POINT('Ctrl Pts',(-0.198020627129986,6.00662573148117,
3.55068011444686));
#13720=CARTESIAN_POINT('Ctrl Pts',(-0.10076495902483,5.99779697154375,3.58474829480414));
#13721=CARTESIAN_POINT('Ctrl Pts',(0.0156022323485835,5.98602915164187,
3.65776634877876));
#13722=CARTESIAN_POINT('Ctrl Pts',(0.124579597342358,5.97132617166562,3.79450200461182));
#13723=CARTESIAN_POINT('Ctrl Pts',(0.171307599715364,5.95369881069723,3.99892400350196));
#13724=CARTESIAN_POINT('Ctrl Pts',(0.124586125732732,5.93609064773941,4.20309708206352));
#13725=CARTESIAN_POINT('Ctrl Pts',(0.00506039749480362,5.91997078621416,
4.35300358200538));
#13726=CARTESIAN_POINT('Ctrl Pts',(-0.145693538275405,5.9053358357862,4.43620069859275));
#13727=CARTESIAN_POINT('Ctrl Pts',(-0.298307108656463,5.89217919980634,
4.46217466683996));
#13728=CARTESIAN_POINT('Ctrl Pts',(-0.4506139703325,5.87903967195749,4.43616034004319));
#13729=CARTESIAN_POINT('Ctrl Pts',(-0.631049677432172,5.86154513447298,
4.33689323122855));
#13730=CARTESIAN_POINT('Ctrl Pts',(-0.773616196183908,5.83972276022349,
4.11032978657596));
#13731=CARTESIAN_POINT('Ctrl Pts',(-0.737476573839881,5.81362592603361,
3.7917862723857));
#13732=CARTESIAN_POINT('Ctrl Pts',(-0.511745890186628,5.78762592348582,
3.5663291033827));
#13733=CARTESIAN_POINT('Ctrl Pts',(-0.195652728007556,5.76173371775045,
3.53089989430616));
#13734=CARTESIAN_POINT('Ctrl Pts',(0.0271465436298084,5.74025186815025,
3.67148645494915));
#13735=CARTESIAN_POINT('Ctrl Pts',(0.124242507955019,5.723131520039,3.84810446118424));
#13736=CARTESIAN_POINT('Ctrl Pts',(0.141141112031897,5.7145929194544,3.94698799978555));
#13737=CARTESIAN_POINT('Ctrl Pts',(0.141147803406803,5.71032999235489,3.99658474166685));
#13738=CARTESIAN_POINT('Ctrl Pts',(0.0442569588189985,7.0373337582885,3.99890379365327));
#13739=CARTESIAN_POINT('Ctrl Pts',(0.044251720623501,7.03399662424325,4.0377294577401));
#13740=CARTESIAN_POINT('Ctrl Pts',(0.0310421174065812,7.02733438487718,
4.11487645730137));
#13741=CARTESIAN_POINT('Ctrl Pts',(-0.044520373619987,7.0140191496109,4.25222378524957));
#13742=CARTESIAN_POINT('Ctrl Pts',(-0.217092875989633,6.9973934512664,4.36083736886208));
#13743=CARTESIAN_POINT('Ctrl Pts',(-0.460362141449961,6.97746421899541,
4.33337109400074));
#13744=CARTESIAN_POINT('Ctrl Pts',(-0.633229581407061,6.95754409339033,
4.16044956838266));
#13745=CARTESIAN_POINT('Ctrl Pts',(-0.660649519608787,6.93762277079198,
3.9173921089824));
#13746=CARTESIAN_POINT('Ctrl Pts',(-0.530497743214058,6.91768886249792,
3.71017764393557));
#13747=CARTESIAN_POINT('Ctrl Pts',(-0.299219066943147,6.89773161738857,
3.62914591381445));
#13748=CARTESIAN_POINT('Ctrl Pts',(-0.0762481443875615,6.8784802155694,
3.70724406195172));
#13749=CARTESIAN_POINT('Ctrl Pts',(0.0504447451103739,6.85993019956411,
3.89325360676551));
#13750=CARTESIAN_POINT('Ctrl Pts',(0.0507270478770132,6.8420804059587,4.1097457930552));
#13751=CARTESIAN_POINT('Ctrl Pts',(-0.061345173924128,6.82567116808314,
4.27427218667378));
#13752=CARTESIAN_POINT('Ctrl Pts',(-0.221824833436464,6.81071112770432,
4.35136044287204));
#13753=CARTESIAN_POINT('Ctrl Pts',(-0.382377722888624,6.79721237823048,
4.35143578641661));
#13754=CARTESIAN_POINT('Ctrl Pts',(-0.527460201032351,6.78367653739436,
4.2815814647059));
#13755=CARTESIAN_POINT('Ctrl Pts',(-0.628251688517972,6.77009810114687,
4.1553667808244));
#13756=CARTESIAN_POINT('Ctrl Pts',(-0.664300918515711,6.75647582308053,
3.99739333351463));
#13757=CARTESIAN_POINT('Ctrl Pts',(-0.628247832683737,6.74280717262616,
3.83886658894804));
#13758=CARTESIAN_POINT('Ctrl Pts',(-0.526580608007555,6.72908872568232,
3.71121541326947));
#13759=CARTESIAN_POINT('Ctrl Pts',(-0.379000812565982,6.71531747846208,
3.64009790518248));
#13760=CARTESIAN_POINT('Ctrl Pts',(-0.214574935364114,6.70149202624025,
3.64001889290798));
#13761=CARTESIAN_POINT('Ctrl Pts',(-0.0656866478755031,6.68760926695514,
3.71161277891696));
#13762=CARTESIAN_POINT('Ctrl Pts',(0.0376362054416423,6.6736673626485,3.84121263629532));
#13763=CARTESIAN_POINT('Ctrl Pts',(0.0792800261450241,6.65810712777825,
4.02168616321321));
#13764=CARTESIAN_POINT('Ctrl Pts',(0.0179396503705256,6.64090166096957,
4.22114376447229));
#13765=CARTESIAN_POINT('Ctrl Pts',(-0.146252315151375,6.62358638474026,
4.35224015227077));
#13766=CARTESIAN_POINT('Ctrl Pts',(-0.295254695663572,6.61092185793103,
4.37448789694979));
#13767=CARTESIAN_POINT('Ctrl Pts',(-0.423135906675798,6.59980383275673,
4.35525987816847));
#13768=CARTESIAN_POINT('Ctrl Pts',(-0.542699558880315,6.58864825053648,
4.29779214729782));
#13769=CARTESIAN_POINT('Ctrl Pts',(-0.649748287956536,6.5742326725394,4.16376617529517));
#13770=CARTESIAN_POINT('Ctrl Pts',(-0.687992729133971,6.55974144076396,
3.99575416152389));
#13771=CARTESIAN_POINT('Ctrl Pts',(-0.643465150667448,6.54274640684286,
3.79858751496941));
#13772=CARTESIAN_POINT('Ctrl Pts',(-0.474396005533634,6.52319303697642,
3.62818230613942));
#13773=CARTESIAN_POINT('Ctrl Pts',(-0.233899438524157,6.50348113431911,
3.60112665283043));
#13774=CARTESIAN_POINT('Ctrl Pts',(-0.0477706845000143,6.48611482218327,
3.69107139148393));
#13775=CARTESIAN_POINT('Ctrl Pts',(0.06333604123178,6.47114764580443,3.83007984654435));
#13776=CARTESIAN_POINT('Ctrl Pts',(0.099942513815026,6.45735180967165,3.99015866708828));
#13777=CARTESIAN_POINT('Ctrl Pts',(0.0750991629903671,6.44474937141879,
4.13630617444996));
#13778=CARTESIAN_POINT('Ctrl Pts',(0.0103545698946879,6.43336007312552,
4.25368042396433));
#13779=CARTESIAN_POINT('Ctrl Pts',(-0.0899993132508311,6.42192347736188,
4.34320250093748));
#13780=CARTESIAN_POINT('Ctrl Pts',(-0.256324344794604,6.40661143299051,
4.4126505577667));
#13781=CARTESIAN_POINT('Ctrl Pts',(-0.491200921321888,6.38735277795623,
4.3867749537966));
#13782=CARTESIAN_POINT('Ctrl Pts',(-0.693833157267625,6.36405139407747,
4.18461691050123));
#13783=CARTESIAN_POINT('Ctrl Pts',(-0.726414474840098,6.34056093669188,
3.89809595710794));
#13784=CARTESIAN_POINT('Ctrl Pts',(-0.57209606869426,6.31688067742868,3.65157253476251));
#13785=CARTESIAN_POINT('Ctrl Pts',(-0.34174487852591,6.2969914003347,3.57092118513008));
#13786=CARTESIAN_POINT('Ctrl Pts',(-0.156064544641843,6.28098618732206,
3.60283127144748));
#13787=CARTESIAN_POINT('Ctrl Pts',(-0.0181211835377871,6.26759749754076,
3.67880681109718));
#13788=CARTESIAN_POINT('Ctrl Pts',(0.0917071518592229,6.25280461900015,
3.81633040921865));
#13789=CARTESIAN_POINT('Ctrl Pts',(0.134725986725988,6.23658646287139,4.0044321517635));
#13790=CARTESIAN_POINT('Ctrl Pts',(0.0952665525924826,6.2216474183188,4.17770434573801));
#13791=CARTESIAN_POINT('Ctrl Pts',(0.00234826205902896,6.20800987537027,
4.30855288182894));
#13792=CARTESIAN_POINT('Ctrl Pts',(-0.115777655276309,6.19569304278798,
4.39248379346406));
#13793=CARTESIAN_POINT('Ctrl Pts',(-0.255507423162007,6.18333388843454,
4.43275482656015));
#13794=CARTESIAN_POINT('Ctrl Pts',(-0.417424148324254,6.1695541663508,4.42379163882968));
#13795=CARTESIAN_POINT('Ctrl Pts',(-0.580494199072148,6.15433738090676,
4.34530507136999));
#13796=CARTESIAN_POINT('Ctrl Pts',(-0.704336977323806,6.13766622912363,
4.19035189958122));
#13797=CARTESIAN_POINT('Ctrl Pts',(-0.748674915963105,6.12092336607669,
3.99618742403465));
#13798=CARTESIAN_POINT('Ctrl Pts',(-0.704328759622937,6.10411386533969,
3.80118099794721));
#13799=CARTESIAN_POINT('Ctrl Pts',(-0.579138032632301,6.08723770701643,
3.64420072065554));
#13800=CARTESIAN_POINT('Ctrl Pts',(-0.427899020685579,6.07312085586337,
3.57125725585403));
#13801=CARTESIAN_POINT('Ctrl Pts',(-0.296498016849044,6.06179556804166,
3.55652395581677));
#13802=CARTESIAN_POINT('Ctrl Pts',(-0.197792520819203,6.05328612269475,
3.56760248202455));
#13803=CARTESIAN_POINT('Ctrl Pts',(-0.103880776642972,6.04476202684289,
3.60048749552585));
#13804=CARTESIAN_POINT('Ctrl Pts',(0.00871742473144576,6.03337695875632,
3.67111939944296));
#13805=CARTESIAN_POINT('Ctrl Pts',(0.114534197432594,6.01911078308422,3.80376795494684));
#13806=CARTESIAN_POINT('Ctrl Pts',(0.160165391665353,6.00193635608825,4.00294447276823));
#13807=CARTESIAN_POINT('Ctrl Pts',(0.114532721808726,5.98470952374257,4.20275174445739));
#13808=CARTESIAN_POINT('Ctrl Pts',(-0.00284531791589128,5.9688722885223,
4.3501044912035));
#13809=CARTESIAN_POINT('Ctrl Pts',(-0.151509186623747,5.9544396588332,4.43219617802463));
#13810=CARTESIAN_POINT('Ctrl Pts',(-0.302485556876914,5.94142572331473,
4.45793192009972));
#13811=CARTESIAN_POINT('Ctrl Pts',(-0.453653070305428,5.92838747414629,
4.43214963221505));
#13812=CARTESIAN_POINT('Ctrl Pts',(-0.633313395400228,5.91097204664598,
4.33337553358166));
#13813=CARTESIAN_POINT('Ctrl Pts',(-0.776152268672977,5.88915102619383,
4.10690588901937));
#13814=CARTESIAN_POINT('Ctrl Pts',(-0.740125674897743,5.86288681368008,
3.78621135475587));
#13815=CARTESIAN_POINT('Ctrl Pts',(-0.511714727939696,5.8365560405257,3.55759037145094));
#13816=CARTESIAN_POINT('Ctrl Pts',(-0.189550345441767,5.81016809980556,
3.52112644113214));
#13817=CARTESIAN_POINT('Ctrl Pts',(0.0391040166061708,5.78814007529024,
3.66511438089066));
#13818=CARTESIAN_POINT('Ctrl Pts',(0.139214121292207,5.77049985171582,3.84708655092079));
#13819=CARTESIAN_POINT('Ctrl Pts',(0.156700985320598,5.76167201173322,3.9493235059236));
#13820=CARTESIAN_POINT('Ctrl Pts',(0.156707905565383,5.75726327669175,4.00061664061033));
#13821=CARTESIAN_POINT('Ctrl Pts',(0.0751457037399773,6.99854476807283,
3.99557397917139));
#13822=CARTESIAN_POINT('Ctrl Pts',(0.075140007219866,6.99491564594273,4.03779675921048));
#13823=CARTESIAN_POINT('Ctrl Pts',(0.0607581710523704,6.98766756923154,
4.1217301725566));
#13824=CARTESIAN_POINT('Ctrl Pts',(-0.0212194890442437,6.97323144469361,
4.27063232486073));
#13825=CARTESIAN_POINT('Ctrl Pts',(-0.207586513843011,6.9552906871778,4.38769413865131));
#13826=CARTESIAN_POINT('Ctrl Pts',(-0.468424025791189,6.93392328513651,
4.35794023955));
#13827=CARTESIAN_POINT('Ctrl Pts',(-0.652319413050973,6.91271075698153,
4.17355011831035));
#13828=CARTESIAN_POINT('Ctrl Pts',(-0.680999823764982,6.89164674870683,
3.91645876707414));
#13829=CARTESIAN_POINT('Ctrl Pts',(-0.544080453606905,6.87072405599895,
3.69908687220202));
#13830=CARTESIAN_POINT('Ctrl Pts',(-0.3029915213572,6.84993503879299,3.61497227631154));
#13831=CARTESIAN_POINT('Ctrl Pts',(-0.0725787408381743,6.83003719070295,
3.69601298637691));
#13832=CARTESIAN_POINT('Ctrl Pts',(0.0572211404977879,6.81100671844234,
3.88702167820545));
#13833=CARTESIAN_POINT('Ctrl Pts',(0.0572773755168048,6.79282253208309,
4.10760648245781));
#13834=CARTESIAN_POINT('Ctrl Pts',(-0.0562661565167663,6.77622751890747,
4.27390914776326));
#13835=CARTESIAN_POINT('Ctrl Pts',(-0.217603410728839,6.76119500558845,
4.35128302310882));
#13836=CARTESIAN_POINT('Ctrl Pts',(-0.378103579756139,6.74770325553529,
4.3512621445762));
#13837=CARTESIAN_POINT('Ctrl Pts',(-0.522312778460912,6.73424518629264,
4.28171670475117));
#13838=CARTESIAN_POINT('Ctrl Pts',(-0.621904906869197,6.72082120908127,
4.15685139905434));
#13839=CARTESIAN_POINT('Ctrl Pts',(-0.657262086760371,6.70742610962714,
4.00146518682517));
#13840=CARTESIAN_POINT('Ctrl Pts',(-0.621901886731202,6.69405663540931,
3.84640605158284));
#13841=CARTESIAN_POINT('Ctrl Pts',(-0.522899910822995,6.6807105640045,3.72225590441482));
#13842=CARTESIAN_POINT('Ctrl Pts',(-0.380021303489903,6.66738551430775,
3.65350850640738));
#13843=CARTESIAN_POINT('Ctrl Pts',(-0.221699556245957,6.65407642679375,
3.6535238424819));
#13844=CARTESIAN_POINT('Ctrl Pts',(-0.0791142190191431,6.64078122645618,
3.72219044199103));
#13845=CARTESIAN_POINT('Ctrl Pts',(0.0192972475475469,6.62749562655119,
3.8457679781254));
#13846=CARTESIAN_POINT('Ctrl Pts',(0.0586956163165313,6.61274299064652,
4.01696310984453));
#13847=CARTESIAN_POINT('Ctrl Pts',(0.00066375925222291,6.59651620933359,
4.2050275731726));
#13848=CARTESIAN_POINT('Ctrl Pts',(-0.153334584529499,6.58029099014053,
4.32775376427335));
#13849=CARTESIAN_POINT('Ctrl Pts',(-0.292259119428385,6.5684849763937,4.34842537504501));
#13850=CARTESIAN_POINT('Ctrl Pts',(-0.411147701512788,6.55814961736179,
4.33054329311896));
#13851=CARTESIAN_POINT('Ctrl Pts',(-0.521955614976932,6.54781050041763,
4.27721853387123));
#13852=CARTESIAN_POINT('Ctrl Pts',(-0.620725061677617,6.53450259960706,
4.15344094423789));
#13853=CARTESIAN_POINT('Ctrl Pts',(-0.65582099214931,6.52118134802923,3.9989509292853));
#13854=CARTESIAN_POINT('Ctrl Pts',(-0.61495699708586,6.50561562040471,3.81836101275701));
#13855=CARTESIAN_POINT('Ctrl Pts',(-0.460662252093786,6.4877934967267,3.66313033402));
#13856=CARTESIAN_POINT('Ctrl Pts',(-0.242482824178419,6.46991415829505,
3.63876953283619));
#13857=CARTESIAN_POINT('Ctrl Pts',(-0.0743337604068055,6.45422487028971,
3.7201015694052));
#13858=CARTESIAN_POINT('Ctrl Pts',(0.0257354859861971,6.44073974504913,
3.84538128706963));
#13859=CARTESIAN_POINT('Ctrl Pts',(0.0585804358516633,6.4283462329255,3.9892205820693));
#13860=CARTESIAN_POINT('Ctrl Pts',(0.0362872215500701,6.4170485024808,4.1202410123795));
#13861=CARTESIAN_POINT('Ctrl Pts',(-0.0216702917476953,6.40685673434529,
4.22527201055116));
#13862=CARTESIAN_POINT('Ctrl Pts',(-0.111335998722885,6.39664004540801,
4.30523794358292));
#13863=CARTESIAN_POINT('Ctrl Pts',(-0.259711447124339,6.38298245740987,
4.36716519030964));
#13864=CARTESIAN_POINT('Ctrl Pts',(-0.46875010272031,6.36584361765854,4.34403783761716));
#13865=CARTESIAN_POINT('Ctrl Pts',(-0.648586756900391,6.34515613291672,
4.16448041223341));
#13866=CARTESIAN_POINT('Ctrl Pts',(-0.677373174728768,6.32434544881345,
3.91060268518533));
#13867=CARTESIAN_POINT('Ctrl Pts',(-0.540800891160044,6.30339796777644,
3.69254462095115));
#13868=CARTESIAN_POINT('Ctrl Pts',(-0.337234792203235,6.28582440056116,
3.62130867843882));
#13869=CARTESIAN_POINT('Ctrl Pts',(-0.173237146150972,6.27168848386102,
3.64949647834371));
#13870=CARTESIAN_POINT('Ctrl Pts',(-0.051430185488775,6.2598663781925,3.71658825071815));
#13871=CARTESIAN_POINT('Ctrl Pts',(0.04553624276142,6.24680590347271,3.83800936553293));
#13872=CARTESIAN_POINT('Ctrl Pts',(0.0835203927235832,6.23248666293686,
4.00408895192877));
#13873=CARTESIAN_POINT('Ctrl Pts',(0.0486781044779186,6.21929378875258,
4.15710891455627));
#13874=CARTESIAN_POINT('Ctrl Pts',(-0.0334048064306245,6.20724619112471,
4.27270501202057));
#13875=CARTESIAN_POINT('Ctrl Pts',(-0.137798620671507,6.19636086286606,
4.34688345273625));
#13876=CARTESIAN_POINT('Ctrl Pts',(-0.261348178132289,6.18543268369284,
4.38249551422101));
#13877=CARTESIAN_POINT('Ctrl Pts',(-0.404602265285608,6.17324102985752,
4.37457199336662));
#13878=CARTESIAN_POINT('Ctrl Pts',(-0.549002049255003,6.15976710926115,
4.30508999673435));
#13879=CARTESIAN_POINT('Ctrl Pts',(-0.658795353214431,6.14498870842845,
4.16774772662554));
#13880=CARTESIAN_POINT('Ctrl Pts',(-0.698173399037309,6.13012858235954,
3.99542272969115));
#13881=CARTESIAN_POINT('Ctrl Pts',(-0.658783439304685,6.11518723031923,
3.82209155039728));
#13882=CARTESIAN_POINT('Ctrl Pts',(-0.547360330742578,6.10016316209671,
3.68232226746707));
#13883=CARTESIAN_POINT('Ctrl Pts',(-0.412501870305111,6.0875735567346,3.61724796858836));
#13884=CARTESIAN_POINT('Ctrl Pts',(-0.295158341169763,6.07745968950951,
3.60408403079106));
#13885=CARTESIAN_POINT('Ctrl Pts',(-0.20692700197197,6.0698531511466,3.61398247465688));
#13886=CARTESIAN_POINT('Ctrl Pts',(-0.122893280869518,6.06222564151618,
3.64340341424773));
#13887=CARTESIAN_POINT('Ctrl Pts',(-0.0220334947688963,6.05202741453606,
3.70666465199554));
#13888=CARTESIAN_POINT('Ctrl Pts',(0.0729349027491596,6.03922702577368,
3.82565491225774));
#13889=CARTESIAN_POINT('Ctrl Pts',(0.114014005851098,6.02378160903268,4.00475544378273));
#13890=CARTESIAN_POINT('Ctrl Pts',(0.0729309939381365,6.00825150319719,
4.18488477257113));
#13891=CARTESIAN_POINT('Ctrl Pts',(-0.0331103150260445,5.99393771535338,
4.31808397533113));
#13892=CARTESIAN_POINT('Ctrl Pts',(-0.167763499397065,5.98086359359795,
4.39247080088669));
#13893=CARTESIAN_POINT('Ctrl Pts',(-0.304804591381143,5.9690494019362,4.41585679085843));
#13894=CARTESIAN_POINT('Ctrl Pts',(-0.442321747056314,5.95718795428887,
4.39242706556015));
#13895=CARTESIAN_POINT('Ctrl Pts',(-0.606120129125199,5.94131003833698,
4.30241537837807));
#13896=CARTESIAN_POINT('Ctrl Pts',(-0.736935222086037,5.92134505674546,
4.09535276040965));
#13897=CARTESIAN_POINT('Ctrl Pts',(-0.704063817046733,5.897202863713,3.8005784837169));
#13898=CARTESIAN_POINT('Ctrl Pts',(-0.493262956617019,5.87287814300756,
3.58923924816358));
#13899=CARTESIAN_POINT('Ctrl Pts',(-0.194189503439066,5.84837693048783,
3.55511225114028));
#13900=CARTESIAN_POINT('Ctrl Pts',(0.0193738527175865,5.82781135703401,
3.68933048543546));
#13901=CARTESIAN_POINT('Ctrl Pts',(0.113245033351325,5.81127961886183,3.85984437961461));
#13902=CARTESIAN_POINT('Ctrl Pts',(0.129703151080226,5.80298162751628,3.95593314931651));
#13903=CARTESIAN_POINT('Ctrl Pts',(0.129709662131318,5.79883358073614,4.00419332376098));
#13904=CARTESIAN_POINT('Ctrl Pts',(0.124798013448484,6.99868851973232,3.99559303376014));
#13905=CARTESIAN_POINT('Ctrl Pts',(0.124791575197003,6.99458685758227,4.04331354923134));
#13906=CARTESIAN_POINT('Ctrl Pts',(0.108519340653653,6.98638331383568,4.13830928780707));
#13907=CARTESIAN_POINT('Ctrl Pts',(0.0157294368859061,6.97004260916147,
4.30685622612404));
#13908=CARTESIAN_POINT('Ctrl Pts',(-0.195313267658951,6.94972310181207,
4.43944484961639));
#13909=CARTESIAN_POINT('Ctrl Pts',(-0.490725500432085,6.92552221004534,
4.4057409716263));
#13910=CARTESIAN_POINT('Ctrl Pts',(-0.698906971683536,6.90150379307887,
4.19696215792743));
#13911=CARTESIAN_POINT('Ctrl Pts',(-0.731302466905495,6.87767190209846,
3.90610635189342));
#13912=CARTESIAN_POINT('Ctrl Pts',(-0.57652734771189,6.85402790905394,3.66052645769687));
#13913=CARTESIAN_POINT('Ctrl Pts',(-0.304524133193118,6.83057351697921,
3.56572939296188));
#13914=CARTESIAN_POINT('Ctrl Pts',(-0.0451810802227447,6.80817096763108,
3.65706578636171));
#13915=CARTESIAN_POINT('Ctrl Pts',(0.10050224257138,6.78679665612694,3.87162772975011));
#13916=CARTESIAN_POINT('Ctrl Pts',(0.100457763025169,6.76642768238877,4.11869777142394));
#13917=CARTESIAN_POINT('Ctrl Pts',(-0.0264325451155999,6.74789297827438,
4.30435282479636));
#13918=CARTESIAN_POINT('Ctrl Pts',(-0.206109828879609,6.7311512513616,4.39045119843915));
#13919=CARTESIAN_POINT('Ctrl Pts',(-0.384343980705665,6.71616672905262,
4.39036989044689));
#13920=CARTESIAN_POINT('Ctrl Pts',(-0.543993429740019,6.70126503100192,
4.31331397713504));
#13921=CARTESIAN_POINT('Ctrl Pts',(-0.65388167053252,6.68644371689127,4.1754321737649));
#13922=CARTESIAN_POINT('Ctrl Pts',(-0.692721455623035,6.67170290736964,
4.00444785555966));
#13923=CARTESIAN_POINT('Ctrl Pts',(-0.653879336914907,6.6570414842913,3.83444051025451));
#13924=CARTESIAN_POINT('Ctrl Pts',(-0.545657981513214,6.64245786103533,
3.69884639844091));
#13925=CARTESIAN_POINT('Ctrl Pts',(-0.390109756917324,6.62795015317063,
3.62408934269625));
#13926=CARTESIAN_POINT('Ctrl Pts',(-0.218468583985697,6.61351806688075,
3.62418508472824));
#13927=CARTESIAN_POINT('Ctrl Pts',(-0.0645595410678361,6.59915930397135,
3.69840045898558));
#13928=CARTESIAN_POINT('Ctrl Pts',(0.0411765748371212,6.58487294660812,
3.83130376244869));
#13929=CARTESIAN_POINT('Ctrl Pts',(0.083247757435789,6.56907615945228,4.01458173082189));
#13930=CARTESIAN_POINT('Ctrl Pts',(0.0212844204770885,6.55180018803028,
4.2147383509278));
#13931=CARTESIAN_POINT('Ctrl Pts',(-0.141775654108723,6.53462919748218,
4.34442182713541));
#13932=CARTESIAN_POINT('Ctrl Pts',(-0.287926289336259,6.52220689767782,
4.36608503842369));
#13933=CARTESIAN_POINT('Ctrl Pts',(-0.412575975619086,6.51136947179089,
4.34732797703399));
#13934=CARTESIAN_POINT('Ctrl Pts',(-0.528343188394878,6.5005621516852,4.29153814826038));
#13935=CARTESIAN_POINT('Ctrl Pts',(-0.630947515877118,6.48672638390543,
4.16279511909207));
#13936=CARTESIAN_POINT('Ctrl Pts',(-0.667156630704825,6.47294344017427,
4.00298851862108));
#13937=CARTESIAN_POINT('Ctrl Pts',(-0.624997276978197,6.45692653478884,
3.81720227944088));
#13938=CARTESIAN_POINT('Ctrl Pts',(-0.467057927631317,6.4387005619605,3.65873827571917));
#13939=CARTESIAN_POINT('Ctrl Pts',(-0.245834304281332,6.4205698163312,3.63434388139158));
#13940=CARTESIAN_POINT('Ctrl Pts',(-0.0765730344102318,6.40476511714423,
3.71634854532427));
#13941=CARTESIAN_POINT('Ctrl Pts',(0.0235696507731436,6.39125997399593,
3.84186810089354));
#13942=CARTESIAN_POINT('Ctrl Pts',(0.0561947006325922,6.3789107097248,3.98516908431952));
#13943=CARTESIAN_POINT('Ctrl Pts',(0.0340532508098388,6.36770980799088,
4.11504089990853));
#13944=CARTESIAN_POINT('Ctrl Pts',(-0.0232053258500781,6.35764612467795,
4.21871751604287));
#13945=CARTESIAN_POINT('Ctrl Pts',(-0.111393660303079,6.34759820362209,
4.29731940679757));
#13946=CARTESIAN_POINT('Ctrl Pts',(-0.256738526493721,6.33422090775404,
4.35791879870519));
#13947=CARTESIAN_POINT('Ctrl Pts',(-0.460216792556107,6.31753050026247,
4.33514023261262));
#13948=CARTESIAN_POINT('Ctrl Pts',(-0.633672374499552,6.29754795827952,
4.16149374392549));
#13949=CARTESIAN_POINT('Ctrl Pts',(-0.660949637255133,6.27759198565784,
3.91813756683918));
#13950=CARTESIAN_POINT('Ctrl Pts',(-0.53077931166136,6.25765964857123,3.71087969162022));
#13951=CARTESIAN_POINT('Ctrl Pts',(-0.33846821757528,6.24105542601477,3.64383802463471));
#13952=CARTESIAN_POINT('Ctrl Pts',(-0.184444074251402,6.22777510682923,
3.67036091043645));
#13953=CARTESIAN_POINT('Ctrl Pts',(-0.0704339054081569,6.2167058919551,
3.7331989943449));
#13954=CARTESIAN_POINT('Ctrl Pts',(0.0199204368139329,6.20452621499493,
3.84646102936634));
#13955=CARTESIAN_POINT('Ctrl Pts',(0.0551098304872991,6.19123118680399,
4.00065923711283));
#13956=CARTESIAN_POINT('Ctrl Pts',(0.0228302131702101,6.1790331648205,4.14210729423421));
#13957=CARTESIAN_POINT('Ctrl Pts',(-0.0528133398235512,6.16793255456529,
4.24857750065134));
#13958=CARTESIAN_POINT('Ctrl Pts',(-0.148722501496592,6.15793189937884,
4.31668991376579));
#13959=CARTESIAN_POINT('Ctrl Pts',(-0.261896992548591,6.14791939152312,
4.34928384757038));
#13960=CARTESIAN_POINT('Ctrl Pts',(-0.392743709961473,6.13678179173137,
4.34201524293595));
#13961=CARTESIAN_POINT('Ctrl Pts',(-0.524209299176861,6.1245107719564,4.27870091640551));
#13962=CARTESIAN_POINT('Ctrl Pts',(-0.623804592783382,6.11109541704753,
4.1540163818384));
#13963=CARTESIAN_POINT('Ctrl Pts',(-0.659377157185489,6.09765172267441,
3.99811930846562));
#13964=CARTESIAN_POINT('Ctrl Pts',(-0.62379462303483,6.08417214571078,3.8417901780194));
#13965=CARTESIAN_POINT('Ctrl Pts',(-0.523543767573635,6.07065633465871,
3.71610462448052));
#13966=CARTESIAN_POINT('Ctrl Pts',(-0.402545085275045,6.05936021527247,
3.6577583409882));
#13967=CARTESIAN_POINT('Ctrl Pts',(-0.297471872035578,6.0503031208645,3.6459761452668));
#13968=CARTESIAN_POINT('Ctrl Pts',(-0.218558620392158,6.04349971284653,
3.65483446064));
#13969=CARTESIAN_POINT('Ctrl Pts',(-0.143482710344404,6.03668462484246,
3.68112357015323));
#13970=CARTESIAN_POINT('Ctrl Pts',(-0.0534709391286362,6.02758246181735,
3.73758932459396));
#13971=CARTESIAN_POINT('Ctrl Pts',(0.0311419308736091,6.01617355264696,
3.8436466619805));
#13972=CARTESIAN_POINT('Ctrl Pts',(0.0676526336744417,6.00243252914066,
4.00297467696501));
#13973=CARTESIAN_POINT('Ctrl Pts',(0.0311452431252221,5.98863818021461,
4.16294558794561));
#13974=CARTESIAN_POINT('Ctrl Pts',(-0.0629151833074351,5.97594279894951,
4.28106220629714));
#13975=CARTESIAN_POINT('Ctrl Pts',(-0.182207296201302,5.9643598495178,4.34695436925805));
#13976=CARTESIAN_POINT('Ctrl Pts',(-0.303519296564873,5.95390085955684,
4.36765003397419));
#13977=CARTESIAN_POINT('Ctrl Pts',(-0.425166618854115,5.94340734969263,
4.34691962242895));
#13978=CARTESIAN_POINT('Ctrl Pts',(-0.569977269229313,5.92936902647442,
4.26733379692996));
#13979=CARTESIAN_POINT('Ctrl Pts',(-0.685535786419193,5.91172770302844,
4.08438020509818));
#13980=CARTESIAN_POINT('Ctrl Pts',(-0.656499898140925,5.89040718152557,
3.82407675111926));
#13981=CARTESIAN_POINT('Ctrl Pts',(-0.470369297569495,5.86892675166902,
3.63744932630136));
#13982=CARTESIAN_POINT('Ctrl Pts',(-0.206193885052881,5.84728307371841,
3.60727155581054));
#13983=CARTESIAN_POINT('Ctrl Pts',(-0.0173782093166548,5.82910240014456,
3.72587589968568));
#13984=CARTESIAN_POINT('Ctrl Pts',(0.0656915399010325,5.81447418238888,
3.87675001240063));
#13985=CARTESIAN_POINT('Ctrl Pts',(0.0802681551442859,5.80712809467601,
3.9618129389144));
#13986=CARTESIAN_POINT('Ctrl Pts',(0.0802739273614817,5.8034507426456,4.00459684659137));
#13987=CARTESIAN_POINT('Ctrl Pts',(0.155898286953838,7.03728022619773,3.99891425465501));
#13988=CARTESIAN_POINT('Ctrl Pts',(0.155891381493523,7.03288091602972,4.0500977361937));
#13989=CARTESIAN_POINT('Ctrl Pts',(0.138432195279057,7.02407113276436,4.15211258318849));
#13990=CARTESIAN_POINT('Ctrl Pts',(0.038565797916663,7.00647506231035,4.33361879406262));
#13991=CARTESIAN_POINT('Ctrl Pts',(-0.189473518840625,6.9845044451475,4.47714449100908));
#13992=CARTESIAN_POINT('Ctrl Pts',(-0.510457801790799,6.95820850684306,
4.4408079840861));
#13993=CARTESIAN_POINT('Ctrl Pts',(-0.737915267426515,6.93198498747228,
4.21308019321558));
#13994=CARTESIAN_POINT('Ctrl Pts',(-0.773692800313957,6.90584663337165,
3.89414328734837));
#13995=CARTESIAN_POINT('Ctrl Pts',(-0.603422771103904,6.87980181841352,
3.62353526879945));
#13996=CARTESIAN_POINT('Ctrl Pts',(-0.302681629986891,6.85386056759999,
3.51849097457158));
#13997=CARTESIAN_POINT('Ctrl Pts',(-0.0147058400958794,6.8289880657698,
3.6197102775808));
#13998=CARTESIAN_POINT('Ctrl Pts',(0.147679051850326,6.80517848086569,3.85863003203219));
#13999=CARTESIAN_POINT('Ctrl Pts',(0.147745220775547,6.78242389077341,4.1346283406934));
#14000=CARTESIAN_POINT('Ctrl Pts',(0.00570064244535932,6.76166320926415,
4.34263115496595));
#14001=CARTESIAN_POINT('Ctrl Pts',(-0.195956608936766,6.74287152561178,
4.43931546269542));
#14002=CARTESIAN_POINT('Ctrl Pts',(-0.396340311853144,6.72602487978657,
4.43926157585714));
#14003=CARTESIAN_POINT('Ctrl Pts',(-0.576112450455779,6.70924619472044,
4.35252925292814));
#14004=CARTESIAN_POINT('Ctrl Pts',(-0.700030850777678,6.69253636270515,
4.19709322386811));
#14005=CARTESIAN_POINT('Ctrl Pts',(-0.74389769318666,6.67589771458627,4.00409528410642));
#14006=CARTESIAN_POINT('Ctrl Pts',(-0.700031510087649,6.65933220722945,
3.81199668730109));
#14007=CARTESIAN_POINT('Ctrl Pts',(-0.577663754631793,6.64284110408447,
3.65864746207902));
#14008=CARTESIAN_POINT('Ctrl Pts',(-0.401654106030834,6.62642604558861,
3.5740381158214));
#14009=CARTESIAN_POINT('Ctrl Pts',(-0.207333431610751,6.61008845759303,
3.57413426225354));
#14010=CARTESIAN_POINT('Ctrl Pts',(-0.0330325771222907,6.59382967848166,
3.65817267563611));
#14011=CARTESIAN_POINT('Ctrl Pts',(0.0867249114115746,6.57765070813198,
3.8086949886927));
#14012=CARTESIAN_POINT('Ctrl Pts',(0.134373312114564,6.55976435473091,4.01625437067971));
#14013=CARTESIAN_POINT('Ctrl Pts',(0.064200943600672,6.54020522159148,4.24286346201966));
#14014=CARTESIAN_POINT('Ctrl Pts',(-0.12029152798752,6.52078200916156,4.38955907374434));
#14015=CARTESIAN_POINT('Ctrl Pts',(-0.285487765251715,6.50674266719864,
4.41402855850721));
#14016=CARTESIAN_POINT('Ctrl Pts',(-0.426292318861567,6.49450160484564,
4.39284001400122));
#14017=CARTESIAN_POINT('Ctrl Pts',(-0.55695886060963,6.48230474083829,4.32985048339294));
#14018=CARTESIAN_POINT('Ctrl Pts',(-0.672616264480391,6.4667067066286,4.1846858955765));
#14019=CARTESIAN_POINT('Ctrl Pts',(-0.713347999015104,6.45119483968567,
4.00478575277996));
#14020=CARTESIAN_POINT('Ctrl Pts',(-0.66592845882305,6.43319552875216,3.79598496681771));
#14021=CARTESIAN_POINT('Ctrl Pts',(-0.4887581341486,6.4127691710153,3.6183946156295));
#14022=CARTESIAN_POINT('Ctrl Pts',(-0.241498728326516,6.39250941732578,
3.59127281368563));
#14023=CARTESIAN_POINT('Ctrl Pts',(-0.0529425060409864,6.37490536021007,
3.68269376647733));
#14024=CARTESIAN_POINT('Ctrl Pts',(0.0583085954390705,6.35989710487152,
3.82222366005482));
#14025=CARTESIAN_POINT('Ctrl Pts',(0.0944075756390824,6.34621737094437,
3.98102240423213));
#14026=CARTESIAN_POINT('Ctrl Pts',(0.0699085235340198,6.33383941511541,
4.12455298430901));
#14027=CARTESIAN_POINT('Ctrl Pts',(0.00675161232934667,6.32274498294321,
4.23885320140307));
#14028=CARTESIAN_POINT('Ctrl Pts',(-0.090256633454611,6.31169591385856,
4.32527973589332));
#14029=CARTESIAN_POINT('Ctrl Pts',(-0.249726812385787,6.29702309261973,
4.39172521686747));
#14030=CARTESIAN_POINT('Ctrl Pts',(-0.472018088461371,6.27879476792815,
4.36662957913525));
#14031=CARTESIAN_POINT('Ctrl Pts',(-0.660259735570777,6.25708995257749,
4.17779412869095));
#14032=CARTESIAN_POINT('Ctrl Pts',(-0.689429979510665,6.23555833236324,
3.91502853353564));
#14033=CARTESIAN_POINT('Ctrl Pts',(-0.549544978189975,6.21418573888641,
3.69285774823168));
#14034=CARTESIAN_POINT('Ctrl Pts',(-0.344583867661803,6.1965076698517,3.62166594025428));
#14035=CARTESIAN_POINT('Ctrl Pts',(-0.181357894942747,6.1824356292938,3.64982599888188));
#14036=CARTESIAN_POINT('Ctrl Pts',(-0.0609759353177233,6.17074988836366,
3.71622172910107));
#14037=CARTESIAN_POINT('Ctrl Pts',(0.0339738702340465,6.15794530953578,
3.83537372624937));
#14038=CARTESIAN_POINT('Ctrl Pts',(0.070699027192326,6.14403681879006,3.99673460654441));
#14039=CARTESIAN_POINT('Ctrl Pts',(0.0370178729943884,6.13134114386906,
4.14396432017652));
#14040=CARTESIAN_POINT('Ctrl Pts',(-0.0414034061013744,6.11984114333799,
4.25426713362554));
#14041=CARTESIAN_POINT('Ctrl Pts',(-0.140420083399158,6.10952207378331,
4.32454338637078));
#14042=CARTESIAN_POINT('Ctrl Pts',(-0.256779120536252,6.09923333420609,
4.35801270993916));
#14043=CARTESIAN_POINT('Ctrl Pts',(-0.390772964435132,6.08783113368769,
4.3505251901726));
#14044=CARTESIAN_POINT('Ctrl Pts',(-0.524724794165585,6.0753273372258,4.28590847874342));
#14045=CARTESIAN_POINT('Ctrl Pts',(-0.625616062768487,6.06173420831728,
4.15945493331342));
#14046=CARTESIAN_POINT('Ctrl Pts',(-0.661381460593111,6.04818027154711,
4.00223728641184));
#14047=CARTESIAN_POINT('Ctrl Pts',(-0.625613714016865,6.03466962836758,
3.84550094762344));
#14048=CARTESIAN_POINT('Ctrl Pts',(-0.525551501680262,6.0211951913812,3.72022382017239));
#14049=CARTESIAN_POINT('Ctrl Pts',(-0.405502332613917,6.00999486905733,
3.66242421459593));
#14050=CARTESIAN_POINT('Ctrl Pts',(-0.301695807990352,6.00104844401153,
3.65080398560401));
#14051=CARTESIAN_POINT('Ctrl Pts',(-0.223942524395158,5.99434541683584,
3.65954297266594));
#14052=CARTESIAN_POINT('Ctrl Pts',(-0.150177426985106,5.98764995088656,
3.68538608217118));
#14053=CARTESIAN_POINT('Ctrl Pts',(-0.0619734954203226,5.97873123536758,
3.74073401474671));
#14054=CARTESIAN_POINT('Ctrl Pts',(0.0205383989162633,5.96760036580935,
3.84428791195509));
#14055=CARTESIAN_POINT('Ctrl Pts',(0.0558943829569689,5.95426466640533,
3.99898167490483));
#14056=CARTESIAN_POINT('Ctrl Pts',(0.0205364233023731,5.94094754169309,
4.15343929607048));
#14057=CARTESIAN_POINT('Ctrl Pts',(-0.0698977870616078,5.92875347004186,
4.26686649595146));
#14058=CARTESIAN_POINT('Ctrl Pts',(-0.184027799874841,5.91767538066872,
4.32985348664582));
#14059=CARTESIAN_POINT('Ctrl Pts',(-0.299632781229378,5.90771186407747,
4.34953322344785));
#14060=CARTESIAN_POINT('Ctrl Pts',(-0.415115100018854,5.89775216087867,
4.32981503807356));
#14061=CARTESIAN_POINT('Ctrl Pts',(-0.552081340816604,5.88447527420849,
4.25447792316758));
#14062=CARTESIAN_POINT('Ctrl Pts',(-0.660599511459815,5.86788715437798,
4.08221655549765));
#14063=CARTESIAN_POINT('Ctrl Pts',(-0.633187418646854,5.84797211597177,
3.83902623944222));
#14064=CARTESIAN_POINT('Ctrl Pts',(-0.460232598593138,5.82804167779231,
3.66597042270737));
#14065=CARTESIAN_POINT('Ctrl Pts',(-0.21651953940244,5.80808128197822,3.63839308255855));
#14066=CARTESIAN_POINT('Ctrl Pts',(-0.0435016794216495,5.79141903729581,
3.74729104993654));
#14067=CARTESIAN_POINT('Ctrl Pts',(0.0323279853604166,5.77805814895842,
3.88511820484604));
#14068=CARTESIAN_POINT('Ctrl Pts',(0.0455846737864788,5.77137052102706,
3.96257235116211));
#14069=CARTESIAN_POINT('Ctrl Pts',(0.0455899333128428,5.76801979299628,
4.00155617363396));
#14070=CARTESIAN_POINT('Ctrl Pts',(0.144678245631215,7.08554680213199,4.00306133790045));
#14071=CARTESIAN_POINT('Ctrl Pts',(0.144671500355495,7.08124954188956,4.05305752636765));
#14072=CARTESIAN_POINT('Ctrl Pts',(0.127638295897203,7.07264307654079,4.15273372378903));
#14073=CARTESIAN_POINT('Ctrl Pts',(0.0297906758184221,7.05539141371109,
4.33071621748334));
#14074=CARTESIAN_POINT('Ctrl Pts',(-0.194624694461135,7.03376092249549,
4.47227310994897));
#14075=CARTESIAN_POINT('Ctrl Pts',(-0.512793689617035,7.0077016180938,4.43660565671338));
#14076=CARTESIAN_POINT('Ctrl Pts',(-0.739891117513686,6.98155185240586,
4.20969228951669));
#14077=CARTESIAN_POINT('Ctrl Pts',(-0.776134874518362,6.95532017556054,
3.88959979024378));
#14078=CARTESIAN_POINT('Ctrl Pts',(-0.604430469514607,6.92901725042124,
3.61607628645324));
#14079=CARTESIAN_POINT('Ctrl Pts',(-0.298850270112994,6.90265311426136,
3.5089773670217));
#14080=CARTESIAN_POINT('Ctrl Pts',(-0.0041877729162317,6.87721684305035,
3.6122029034201));
#14081=CARTESIAN_POINT('Ctrl Pts',(0.163085243952079,6.8527238294967,3.85787769361227));
#14082=CARTESIAN_POINT('Ctrl Pts',(0.163384882825869,6.82918609064528,4.14338542492333));
#14083=CARTESIAN_POINT('Ctrl Pts',(0.015823003083378,6.80759518268656,4.35983941897781));
#14084=CARTESIAN_POINT('Ctrl Pts',(-0.19485297859053,6.78796098573423,4.46096458777198));
#14085=CARTESIAN_POINT('Ctrl Pts',(-0.405068526852833,6.77028845501068,
4.46099811143608));
#14086=CARTESIAN_POINT('Ctrl Pts',(-0.594442506826705,6.75261759300039,
4.36973390477035));
#14087=CARTESIAN_POINT('Ctrl Pts',(-0.725521830010195,6.73495168097432,
4.20545805379156));
#14088=CARTESIAN_POINT('Ctrl Pts',(-0.772159744972474,6.7172940852679,4.00065424379591));
#14089=CARTESIAN_POINT('Ctrl Pts',(-0.725515499865608,6.69964790652088,
3.79600816012752));
#14090=CARTESIAN_POINT('Ctrl Pts',(-0.594752448164995,6.68201643280477,
3.63200459373353));
#14091=CARTESIAN_POINT('Ctrl Pts',(-0.405927741373564,6.66440258324841,
3.54114672713638));
#14092=CARTESIAN_POINT('Ctrl Pts',(-0.196685934801451,6.64680993881577,
3.5411729761552));
#14093=CARTESIAN_POINT('Ctrl Pts',(-0.00831861674380411,6.62924133491153,
3.63190747468183));
#14094=CARTESIAN_POINT('Ctrl Pts',(0.121572695078818,6.61170024961743,3.79505321054773));
#14095=CARTESIAN_POINT('Ctrl Pts',(0.173479639665487,6.59224330272307,4.02079117854625));
#14096=CARTESIAN_POINT('Ctrl Pts',(0.0970225484155485,6.57088994378068,
4.26823368838363));
#14097=CARTESIAN_POINT('Ctrl Pts',(-0.105126136635525,6.54959621783657,
4.42916044832145));
#14098=CARTESIAN_POINT('Ctrl Pts',(-0.286826829701903,6.53415291663596,
4.4561321994847));
#14099=CARTESIAN_POINT('Ctrl Pts',(-0.441985250736035,6.52066326933656,
4.43278777827631));
#14100=CARTESIAN_POINT('Ctrl Pts',(-0.586261220893134,6.50719630370112,
4.36328940520075));
#14101=CARTESIAN_POINT('Ctrl Pts',(-0.714326528660687,6.48993058540335,
4.20264640858163));
#14102=CARTESIAN_POINT('Ctrl Pts',(-0.759578088890916,6.47271357412861,
4.00301451687559));
#14103=CARTESIAN_POINT('Ctrl Pts',(-0.706890145842292,6.4526901815544,3.77074626745266));
#14104=CARTESIAN_POINT('Ctrl Pts',(-0.509348264358454,6.42989539310044,
3.57253036910641));
#14105=CARTESIAN_POINT('Ctrl Pts',(-0.232673374234872,6.4072213283679,3.54204681697485));
#14106=CARTESIAN_POINT('Ctrl Pts',(-0.0211606489794148,6.38747158289537,
3.64454937174464));
#14107=CARTESIAN_POINT('Ctrl Pts',(0.10385050553,6.37061025692699,3.80127847521638));
#14108=CARTESIAN_POINT('Ctrl Pts',(0.144499767686605,6.35521294411437,3.97996599015471));
#14109=CARTESIAN_POINT('Ctrl Pts',(0.11691297736442,6.34126688370014,4.14166635350243));
#14110=CARTESIAN_POINT('Ctrl Pts',(0.0457037622501119,6.32875467680033,
4.2705620245579));
#14111=CARTESIAN_POINT('Ctrl Pts',(-0.0637765139051123,6.31628241125697,
4.36811362660792));
#14112=CARTESIAN_POINT('Ctrl Pts',(-0.243887986166721,6.29970752541662,
4.44317377591863));
#14113=CARTESIAN_POINT('Ctrl Pts',(-0.495229957712618,6.27909069195944,
4.41484962337697));
#14114=CARTESIAN_POINT('Ctrl Pts',(-0.708286432087431,6.25452486128724,
4.20117890011158));
#14115=CARTESIAN_POINT('Ctrl Pts',(-0.741330918581209,6.23012937021185,
3.90363242728255));
#14116=CARTESIAN_POINT('Ctrl Pts',(-0.582907516210337,6.2059161665878,3.65203300687903));
#14117=CARTESIAN_POINT('Ctrl Pts',(-0.350842144541872,6.18588854891781,
3.57145512299382));
#14118=CARTESIAN_POINT('Ctrl Pts',(-0.16616267347381,6.16996303930852,3.60332715230888));
#14119=CARTESIAN_POINT('Ctrl Pts',(-0.0300193261453657,6.1567431579809,
3.6784240642902));
#14120=CARTESIAN_POINT('Ctrl Pts',(0.0772697082943915,6.14226898651452,
3.81309635659369));
#14121=CARTESIAN_POINT('Ctrl Pts',(0.118711944999288,6.1265634666449,3.99528114055935));
#14122=CARTESIAN_POINT('Ctrl Pts',(0.0806988497789685,6.11224384637075,
4.16130380343939));
#14123=CARTESIAN_POINT('Ctrl Pts',(-0.00764523437737332,6.09928702591431,
4.2855359239597));
#14124=CARTESIAN_POINT('Ctrl Pts',(-0.119061347128016,6.08767307012448,
4.36458894128047));
#14125=CARTESIAN_POINT('Ctrl Pts',(-0.249824643571864,6.07610587445443,
4.40218494533652));
#14126=CARTESIAN_POINT('Ctrl Pts',(-0.400178064050431,6.06330773686186,
4.39376127834984));
#14127=CARTESIAN_POINT('Ctrl Pts',(-0.550214494811022,6.04929754952555,
4.32135094499318));
#14128=CARTESIAN_POINT('Ctrl Pts',(-0.662945002779939,6.03409632303652,
4.1799671043587));
#14129=CARTESIAN_POINT('Ctrl Pts',(-0.702782576913764,6.01898178761487,
4.00466261722736));
#14130=CARTESIAN_POINT('Ctrl Pts',(-0.662935573975121,6.00394761901098,
3.83034152873934));
#14131=CARTESIAN_POINT('Ctrl Pts',(-0.551913042299725,5.98899659078265,
3.69142024206081));
#14132=CARTESIAN_POINT('Ctrl Pts',(-0.419127185826005,5.97660551336272,
3.62754451453377));
#14133=CARTESIAN_POINT('Ctrl Pts',(-0.304612679823387,5.96673442572674,
3.61473293745679));
#14134=CARTESIAN_POINT('Ctrl Pts',(-0.218980861908636,5.95935166909097,
3.62436627546611));
#14135=CARTESIAN_POINT('Ctrl Pts',(-0.137875282342012,5.95198838173858,
3.65278906578636));
#14136=CARTESIAN_POINT('Ctrl Pts',(-0.0410640067172789,5.94219726798964,
3.71355547533596));
#14137=CARTESIAN_POINT('Ctrl Pts',(0.0492362339959224,5.93000589656047,
3.82697125746778));
#14138=CARTESIAN_POINT('Ctrl Pts',(0.0877277228792333,5.91545396739186,
3.99574063387158));
#14139=CARTESIAN_POINT('Ctrl Pts',(0.0492465765145144,5.90097796291407,
4.16356675179509));
#14140=CARTESIAN_POINT('Ctrl Pts',(-0.0486820579380837,5.88777724801351,
4.28628146889304));
#14141=CARTESIAN_POINT('Ctrl Pts',(-0.171751854364245,5.87583082210482,
4.35416544596331));
#14142=CARTESIAN_POINT('Ctrl Pts',(-0.296013425129878,5.86511834632131,
4.37528682708976));
#14143=CARTESIAN_POINT('Ctrl Pts',(-0.419716281141755,5.85444563424213,
4.35413476774134));
#14144=CARTESIAN_POINT('Ctrl Pts',(-0.565929655577575,5.84026767787951,
4.27365549771028));
#14145=CARTESIAN_POINT('Ctrl Pts',(-0.680990719323017,5.8226369137051,4.09054212894091));
#14146=CARTESIAN_POINT('Ctrl Pts',(-0.651757681535579,5.80162737226418,
3.83412076912136));
#14147=CARTESIAN_POINT('Ctrl Pts',(-0.470477481012713,5.78075525660051,
3.65319906029932));
#14148=CARTESIAN_POINT('Ctrl Pts',(-0.217264499890463,5.76001348508868,
3.62489033715765));
#14149=CARTESIAN_POINT('Ctrl Pts',(-0.0390539840425255,5.74283038603375,
3.7373503101674));
#14150=CARTESIAN_POINT('Ctrl Pts',(0.0385809790069335,5.72913985701358,
3.87858381898698));
#14151=CARTESIAN_POINT('Ctrl Pts',(0.0520898426589243,5.722316450254,3.95760322649394));
#14152=CARTESIAN_POINT('Ctrl Pts',(0.0520952028928984,5.71890156362907,
3.99733349786329));
#14153=CARTESIAN_POINT('Ctrl Pts',(0.1149593871984,7.09981632447119,4.00428381887363));
#14154=CARTESIAN_POINT('Ctrl Pts',(0.114953085439515,7.0958016186183,4.05099264708923));
#14155=CARTESIAN_POINT('Ctrl Pts',(0.0990499949612588,7.08776451642407,
4.1440749819009));
#14156=CARTESIAN_POINT('Ctrl Pts',(0.00756609025685691,7.07163054708052,
4.3105312207836));
#14157=CARTESIAN_POINT('Ctrl Pts',(-0.20265191966924,7.05136317960048,4.4432442233264));
#14158=CARTESIAN_POINT('Ctrl Pts',(-0.501576002622839,7.02688068565122,
4.40988522403664));
#14159=CARTESIAN_POINT('Ctrl Pts',(-0.715649296673727,7.00224333371635,
4.19621127354387));
#14160=CARTESIAN_POINT('Ctrl Pts',(-0.750065379754911,6.977454834481,3.89375410180805));
#14161=CARTESIAN_POINT('Ctrl Pts',(-0.587448639243598,6.95252105745876,
3.63437652438941));
#14162=CARTESIAN_POINT('Ctrl Pts',(-0.296883906961772,6.92744748855256,
3.53234593196161));
#14163=CARTESIAN_POINT('Ctrl Pts',(-0.0156214196491875,6.90317435214424,
3.63068646565069));
#14164=CARTESIAN_POINT('Ctrl Pts',(0.144662679260828,6.87972358982664,3.86584230232094));
#14165=CARTESIAN_POINT('Ctrl Pts',(0.145088543148844,6.85711434464457,4.14009778924436));
#14166=CARTESIAN_POINT('Ctrl Pts',(0.00298259309759907,6.83630747956724,
4.3487833250613));
#14167=CARTESIAN_POINT('Ctrl Pts',(-0.200629153718379,6.8173312082382,4.44659816529074));
#14168=CARTESIAN_POINT('Ctrl Pts',(-0.404350038818084,6.80020649499647,
4.44669337921948));
#14169=CARTESIAN_POINT('Ctrl Pts',(-0.588383432588771,6.78303663281808,
4.35806872308743));
#14170=CARTESIAN_POINT('Ctrl Pts',(-0.716130694480413,6.76582937646054,
4.19807595671414));
#14171=CARTESIAN_POINT('Ctrl Pts',(-0.76174697024645,6.74858383891329,3.99803802216038));
#14172=CARTESIAN_POINT('Ctrl Pts',(-0.716126250508271,6.7313025559897,3.79758613790949));
#14173=CARTESIAN_POINT('Ctrl Pts',(-0.58775583974693,6.71398953196761,3.63647816172447));
#14174=CARTESIAN_POINT('Ctrl Pts',(-0.401838339917565,6.69664899601872,
3.54694262619554));
#14175=CARTESIAN_POINT('Ctrl Pts',(-0.195214549156962,6.67928042967714,
3.54690060253338));
#14176=CARTESIAN_POINT('Ctrl Pts',(-0.00865722368073337,6.66188873083374,
3.63668289231812));
#14177=CARTESIAN_POINT('Ctrl Pts',(0.120374244388054,6.64447474921385,3.79864518662284));
#14178=CARTESIAN_POINT('Ctrl Pts',(0.172141661215916,6.62510839439489,4.02339166080862));
#14179=CARTESIAN_POINT('Ctrl Pts',(0.095889564871484,6.60377546807264,4.27065330650525));
#14180=CARTESIAN_POINT('Ctrl Pts',(-0.106719746155468,6.58242925442276,
4.4321448062933));
#14181=CARTESIAN_POINT('Ctrl Pts',(-0.289520583900008,6.5668956717895,4.45933997294184));
#14182=CARTESIAN_POINT('Ctrl Pts',(-0.445921222784358,6.55329978788634,
4.4358156174397));
#14183=CARTESIAN_POINT('Ctrl Pts',(-0.591635462985678,6.53970440462415,
4.36567953699744));
#14184=CARTESIAN_POINT('Ctrl Pts',(-0.721389666696936,6.52221950596346,
4.20303067518927));
#14185=CARTESIAN_POINT('Ctrl Pts',(-0.767405188483471,6.50474251981698,
4.000316390915));
#14186=CARTESIAN_POINT('Ctrl Pts',(-0.713830810800694,6.48435445670912,
3.76376923070465));
#14187=CARTESIAN_POINT('Ctrl Pts',(-0.51214130973696,6.46107773227755,3.56109836625548));
#14188=CARTESIAN_POINT('Ctrl Pts',(-0.228267597822158,6.43781873998792,
3.5296222132148));
#14189=CARTESIAN_POINT('Ctrl Pts',(-0.0104681813815427,6.41749488904288,
3.63508347114042));
#14190=CARTESIAN_POINT('Ctrl Pts',(0.118638327797451,6.40008799366429,3.79685627397656));
#14191=CARTESIAN_POINT('Ctrl Pts',(0.160770132095208,6.38415833960461,3.98178426841228));
#14192=CARTESIAN_POINT('Ctrl Pts',(0.132174615335124,6.36969190973263,4.14955144088928));
#14193=CARTESIAN_POINT('Ctrl Pts',(0.0581767737661934,6.35668810557578,
4.2835498059508));
#14194=CARTESIAN_POINT('Ctrl Pts',(-0.0558338873469698,6.34370163075499,
4.38516402527543));
#14195=CARTESIAN_POINT('Ctrl Pts',(-0.243754538377708,6.32640951048581,
4.46351775255043));
#14196=CARTESIAN_POINT('Ctrl Pts',(-0.506762819769542,6.30484691807606,
4.43403489872079));
#14197=CARTESIAN_POINT('Ctrl Pts',(-0.730668971919691,6.27905054023632,
4.20975403365834));
#14198=CARTESIAN_POINT('Ctrl Pts',(-0.765678686873786,6.25335957707319,
3.89618560227291));
#14199=CARTESIAN_POINT('Ctrl Pts',(-0.59828824591992,6.22776564997827,3.63001002509955));
#14200=CARTESIAN_POINT('Ctrl Pts',(-0.35211960915011,6.20653414885713,3.54438589454075));
#14201=CARTESIAN_POINT('Ctrl Pts',(-0.155684959604055,6.18960076014007,
3.57825744186559));
#14202=CARTESIAN_POINT('Ctrl Pts',(-0.010661377238107,6.1755244002249,3.65822950437421));
#14203=CARTESIAN_POINT('Ctrl Pts',(0.103859085093381,6.1600835663691,3.80190427731936));
#14204=CARTESIAN_POINT('Ctrl Pts',(0.148204575463535,6.14329585710035,3.99667156211874));
#14205=CARTESIAN_POINT('Ctrl Pts',(0.107533874360454,6.12796192084666,4.17450217859232));
#14206=CARTESIAN_POINT('Ctrl Pts',(0.0127852845025076,6.11406789381457,
4.3077723562051));
#14207=CARTESIAN_POINT('Ctrl Pts',(-0.106861005480655,6.1015991481364,4.39269001253556));
#14208=CARTESIAN_POINT('Ctrl Pts',(-0.247456764966195,6.0891678153038,4.43312715503312));
#14209=CARTESIAN_POINT('Ctrl Pts',(-0.409327203073403,6.07539362335861,
4.42407672254863));
#14210=CARTESIAN_POINT('Ctrl Pts',(-0.571069625287454,6.06029537121561,
4.34603758409293));
#14211=CARTESIAN_POINT('Ctrl Pts',(-0.692783271109274,6.04389453255034,
4.19344865326311));
#14212=CARTESIAN_POINT('Ctrl Pts',(-0.735861926194011,6.0275588239698,4.00395604220365));
#14213=CARTESIAN_POINT('Ctrl Pts',(-0.692776967423399,6.01129753338503,
3.81531844116176));
#14214=CARTESIAN_POINT('Ctrl Pts',(-0.572513817468236,5.99510729772473,
3.6648179318568));
#14215=CARTESIAN_POINT('Ctrl Pts',(-0.428536498276722,5.98167596786366,
3.5955416477389));
#14216=CARTESIAN_POINT('Ctrl Pts',(-0.304268279887566,5.97096604692344,
3.58164029219959));
#14217=CARTESIAN_POINT('Ctrl Pts',(-0.211302708259727,5.96295150211699,
3.59209575299587));
#14218=CARTESIAN_POINT('Ctrl Pts',(-0.123221561998884,5.95495625976633,
3.62296222963301));
#14219=CARTESIAN_POINT('Ctrl Pts',(-0.0180442464683113,5.9443206556865,
3.68897371165251));
#14220=CARTESIAN_POINT('Ctrl Pts',(0.0800964737981796,5.93107533649748,
3.81222858617156));
#14221=CARTESIAN_POINT('Ctrl Pts',(0.121963800542189,5.91525638154566,3.99573810944841));
#14222=CARTESIAN_POINT('Ctrl Pts',(0.0800951474414264,5.89951422438799,
4.17829694994921));
#14223=CARTESIAN_POINT('Ctrl Pts',(-0.0264610976803377,5.88515352693233,
4.31182517350449));
#14224=CARTESIAN_POINT('Ctrl Pts',(-0.160404840361885,5.87215362307701,
4.38570130500428));
#14225=CARTESIAN_POINT('Ctrl Pts',(-0.295639561854143,5.86049817284501,
4.40868318905617));
#14226=CARTESIAN_POINT('Ctrl Pts',(-0.430262394364154,5.8488860820304,4.38565877817388));
#14227=CARTESIAN_POINT('Ctrl Pts',(-0.589366688691013,5.83346068619404,
4.29807824715954));
#14228=CARTESIAN_POINT('Ctrl Pts',(-0.714505317186666,5.81429088075568,
4.09887385317267));
#14229=CARTESIAN_POINT('Ctrl Pts',(-0.68268303776338,5.79145791366774,3.82012733243894));
#14230=CARTESIAN_POINT('Ctrl Pts',(-0.485773655554561,5.7687981740651,3.62368921351975));
#14231=CARTESIAN_POINT('Ctrl Pts',(-0.211134005665917,5.74630660226991,
3.59306391087273));
#14232=CARTESIAN_POINT('Ctrl Pts',(-0.0182181343487706,5.72770693474824,
3.71490466632272));
#14233=CARTESIAN_POINT('Ctrl Pts',(0.0657101590335888,5.71290424256539,
3.86762790031566));
#14234=CARTESIAN_POINT('Ctrl Pts',(0.0802918585875821,5.70553413368605,
3.95299047765578));
#14235=CARTESIAN_POINT('Ctrl Pts',(0.0802976428954483,5.7018490789545,3.99586400189706));
#14236=CARTESIAN_POINT('Ctrl Pts',(0.0999994223174587,7.09981632447119,
4.00428180053801));
#14237=CARTESIAN_POINT('Ctrl Pts',(0.0999933436797077,7.09594376396835,
4.04933684813297));
#14238=CARTESIAN_POINT('Ctrl Pts',(0.0846594327171957,7.08819408394972,
4.13908992957458));
#14239=CARTESIAN_POINT('Ctrl Pts',(-0.00357043069494361,7.07263318914228,
4.29963340285418));
#14240=CARTESIAN_POINT('Ctrl Pts',(-0.206356294917572,7.05308143195573,
4.42766373470968));
#14241=CARTESIAN_POINT('Ctrl Pts',(-0.494863120131574,7.02945164505109,
4.39548903188326));
#14242=CARTESIAN_POINT('Ctrl Pts',(-0.701612481834811,7.00565862484048,
4.18915927264886));
#14243=CARTESIAN_POINT('Ctrl Pts',(-0.734902354617378,6.98170298771966,
3.89687986754614));
#14244=CARTESIAN_POINT('Ctrl Pts',(-0.577665286755769,6.9575878275568,3.64601239877861));
#14245=CARTESIAN_POINT('Ctrl Pts',(-0.296425446296891,6.93331589731144,
3.54721069783272));
#14246=CARTESIAN_POINT('Ctrl Pts',(-0.0238970429973844,6.90979548741706,
3.64245102870328));
#14247=CARTESIAN_POINT('Ctrl Pts',(0.131586191166419,6.88704931445005,3.8704985271515));
#14248=CARTESIAN_POINT('Ctrl Pts',(0.132036205657411,6.86509836852865,4.13674945418924));
#14249=CARTESIAN_POINT('Ctrl Pts',(-0.0060413687179679,6.84487478558125,
4.33958298894643));
#14250=CARTESIAN_POINT('Ctrl Pts',(-0.204116844890033,6.82641141958407,
4.43475944317313));
#14251=CARTESIAN_POINT('Ctrl Pts',(-0.402473369433673,6.80973569344043,
4.43486896119673));
#14252=CARTESIAN_POINT('Ctrl Pts',(-0.581827228221285,6.79300305116116,
4.34852221416367));
#14253=CARTESIAN_POINT('Ctrl Pts',(-0.706454134874152,6.7762153628094,4.192464816352));
#14254=CARTESIAN_POINT('Ctrl Pts',(-0.751016294559626,6.75937457420164,
3.99715087739011));
#14255=CARTESIAN_POINT('Ctrl Pts',(-0.706447662037028,6.74248271608976,
3.80123388795173));
#14256=CARTESIAN_POINT('Ctrl Pts',(-0.580873534358325,6.72554188917784,
3.64359934962882));
#14257=CARTESIAN_POINT('Ctrl Pts',(-0.398793807750649,6.70855427056295,
3.55588854173989));
#14258=CARTESIAN_POINT('Ctrl Pts',(-0.196213186746174,6.69152210478501,
3.55582569363604));
#14259=CARTESIAN_POINT('Ctrl Pts',(-0.0130963934752721,6.67444770586136,
3.64392728654252));
#14260=CARTESIAN_POINT('Ctrl Pts',(0.113707820363769,6.65733344528682,3.80305624025719));
#14261=CARTESIAN_POINT('Ctrl Pts',(0.164656362590817,6.63827601697293,4.02413741573514));
#14262=CARTESIAN_POINT('Ctrl Pts',(0.0896082709820025,6.61726302509207,
4.2676978223342));
#14263=CARTESIAN_POINT('Ctrl Pts',(-0.110245732077343,6.59619863179822,
4.4270642600818));
#14264=CARTESIAN_POINT('Ctrl Pts',(-0.290838098938005,6.58084997747224,
4.45395573001046));
#14265=CARTESIAN_POINT('Ctrl Pts',(-0.445467117475853,6.56740673782488,
4.43069910759464));
#14266=CARTESIAN_POINT('Ctrl Pts',(-0.589663880409842,6.55395079532829,
4.36131796304211));
#14267=CARTESIAN_POINT('Ctrl Pts',(-0.718225707768932,6.53662851071928,
4.20020661739991));
#14268=CARTESIAN_POINT('Ctrl Pts',(-0.763898158866166,6.51928717897976,
3.99912848715837));
#14269=CARTESIAN_POINT('Ctrl Pts',(-0.710721419612997,6.49903664059857,
3.764202830041));
#14270=CARTESIAN_POINT('Ctrl Pts',(-0.510149997687367,6.47587070043553,
3.56253207697483));
#14271=CARTESIAN_POINT('Ctrl Pts',(-0.227250362890276,6.45268625633124,
3.53107252428385));
#14272=CARTESIAN_POINT('Ctrl Pts',(-0.00982453983942397,6.43239259089565,
3.63631313688574));
#14273=CARTESIAN_POINT('Ctrl Pts',(0.119224416062016,6.414995879623,3.79796488057796));
#14274=CARTESIAN_POINT('Ctrl Pts',(0.161414220224748,6.39904954972701,3.98302626625864));
#14275=CARTESIAN_POINT('Ctrl Pts',(0.132781651753175,6.38455548538367,4.15109736344141));
#14276=CARTESIAN_POINT('Ctrl Pts',(0.058591217696994,6.37151403493753,4.28547086198332));
#14277=CARTESIAN_POINT('Ctrl Pts',(-0.0558362639783319,6.35847699034469,
4.38747481451575));
#14278=CARTESIAN_POINT('Ctrl Pts',(-0.244624220570673,6.34110173177432,
4.46620946091905));
#14279=CARTESIAN_POINT('Ctrl Pts',(-0.509258386493358,6.31939963958705,
4.43663450707748));
#14280=CARTESIAN_POINT('Ctrl Pts',(-0.735030443095589,6.29339375292805,
4.21063569075453));
#14281=CARTESIAN_POINT('Ctrl Pts',(-0.770492148406669,6.2674338232997,3.89395438143295));
#14282=CARTESIAN_POINT('Ctrl Pts',(-0.601210048531917,6.24152902186401,
3.62457992816658));
#14283=CARTESIAN_POINT('Ctrl Pts',(-0.351688619951789,6.21999512440529,
3.53770552245775));
#14284=CARTESIAN_POINT('Ctrl Pts',(-0.152299417857812,6.20280445728418,
3.57207084012085));
#14285=CARTESIAN_POINT('Ctrl Pts',(-0.00495835013055459,6.18850033974624,
3.65330634586973));
#14286=CARTESIAN_POINT('Ctrl Pts',(0.111522803781729,6.17279483671223,3.79940640678234));
#14287=CARTESIAN_POINT('Ctrl Pts',(0.156701474788417,6.15570021231953,3.99770463755195));
#14288=CARTESIAN_POINT('Ctrl Pts',(0.115262604711903,6.14006777305336,4.17897821875209));
#14289=CARTESIAN_POINT('Ctrl Pts',(0.0185932180471106,6.12588811043834,
4.31497113433199));
#14290=CARTESIAN_POINT('Ctrl Pts',(-0.103590553659916,6.11315178814851,
4.4016989608744));
#14291=CARTESIAN_POINT('Ctrl Pts',(-0.247293954733903,6.1004417858412,4.44304193852122));
#14292=CARTESIAN_POINT('Ctrl Pts',(-0.412869049658234,6.08634982725544,
4.43379507168706));
#14293=CARTESIAN_POINT('Ctrl Pts',(-0.578482300908516,6.07088880084204,
4.3539190346138));
#14294=CARTESIAN_POINT('Ctrl Pts',(-0.703246723757797,6.05407432044984,
4.19753682982269));
#14295=CARTESIAN_POINT('Ctrl Pts',(-0.747469580607062,6.03731392465469,
4.00314057125818));
#14296=CARTESIAN_POINT('Ctrl Pts',(-0.703238625925696,6.02060951959296,
3.80940575329504));
#14297=CARTESIAN_POINT('Ctrl Pts',(-0.579634776479789,6.00396293095479,
3.65467865258803));
#14298=CARTESIAN_POINT('Ctrl Pts',(-0.431500759601328,5.99014040360805,
3.58338254073736));
#14299=CARTESIAN_POINT('Ctrl Pts',(-0.303561319206374,5.97911298339926,
3.56906449106088));
#14300=CARTESIAN_POINT('Ctrl Pts',(-0.207808748835976,5.97085791464426,
3.57983145987356));
#14301=CARTESIAN_POINT('Ctrl Pts',(-0.117044922248722,5.96261853714979,
3.6116348383249));
#14302=CARTESIAN_POINT('Ctrl Pts',(-0.00861997369778145,5.95165386736835,
3.67968231581426));
#14303=CARTESIAN_POINT('Ctrl Pts',(0.0926329081004657,5.93798817658918,
3.80681756846826));
#14304=CARTESIAN_POINT('Ctrl Pts',(0.135870644163702,5.92165495155963,3.99626375633351));
#14305=CARTESIAN_POINT('Ctrl Pts',(0.0926387969430078,5.90538860209907,
4.18487776410349));
#14306=CARTESIAN_POINT('Ctrl Pts',(-0.0175125738479973,5.89054016294629,
4.32293582509909));
#14307=CARTESIAN_POINT('Ctrl Pts',(-0.156061008534171,5.87709197920747,
4.39936287338782));
#14308=CARTESIAN_POINT('Ctrl Pts',(-0.296018497756522,5.86502791432804,
4.42315611503599));
#14309=CARTESIAN_POINT('Ctrl Pts',(-0.435406476921251,5.8530035361086,4.39932451423293));
#14310=CARTESIAN_POINT('Ctrl Pts',(-0.600212844195293,5.83702437044493,
4.30861645270809));
#14311=CARTESIAN_POINT('Ctrl Pts',(-0.729945333339283,5.81715142573852,
4.10216892170714));
#14312=CARTESIAN_POINT('Ctrl Pts',(-0.696976009348358,5.7934671926544,3.81306008549607));
#14313=CARTESIAN_POINT('Ctrl Pts',(-0.492652698548329,5.76994854996481,
3.60918617550531));
#14314=CARTESIAN_POINT('Ctrl Pts',(-0.207515825799976,5.74659510021081,
3.57736699868709));
#14315=CARTESIAN_POINT('Ctrl Pts',(-0.00714719245692835,5.72727465695078,
3.70390131122158));
#14316=CARTESIAN_POINT('Ctrl Pts',(0.0800330609517386,5.71189866882786,
3.86253474741929));
#14317=CARTESIAN_POINT('Ctrl Pts',(0.0951821641861108,5.70424160396714,
3.95121652410011));
#14318=CARTESIAN_POINT('Ctrl Pts',(0.0951881709252366,5.70041484319491,
3.99573871784903));
#14319=CARTESIAN_POINT('',(0.0999994223174587,7.09981632447119,4.00428180053802));
#14320=CARTESIAN_POINT('Origin',(0.1,7.05,4.));
#14321=CARTESIAN_POINT('',(0.0951881709252366,5.70041484319491,3.99573871784901));
#14322=CARTESIAN_POINT('Ctrl Pts',(0.0999994223174587,7.09981632447119,
4.00428180053801));
#14323=CARTESIAN_POINT('Ctrl Pts',(0.0999933436797077,7.09594376396835,
4.04933684813297));
#14324=CARTESIAN_POINT('Ctrl Pts',(0.0846594327171957,7.08819408394972,
4.13908992957458));
#14325=CARTESIAN_POINT('Ctrl Pts',(-0.00357043069494361,7.07263318914228,
4.29963340285418));
#14326=CARTESIAN_POINT('Ctrl Pts',(-0.206356294917572,7.05308143195573,
4.42766373470968));
#14327=CARTESIAN_POINT('Ctrl Pts',(-0.494863120131574,7.02945164505109,
4.39548903188326));
#14328=CARTESIAN_POINT('Ctrl Pts',(-0.701612481834811,7.00565862484048,
4.18915927264886));
#14329=CARTESIAN_POINT('Ctrl Pts',(-0.734902354617378,6.98170298771966,
3.89687986754614));
#14330=CARTESIAN_POINT('Ctrl Pts',(-0.577665286755769,6.9575878275568,3.64601239877861));
#14331=CARTESIAN_POINT('Ctrl Pts',(-0.296425446296891,6.93331589731144,
3.54721069783272));
#14332=CARTESIAN_POINT('Ctrl Pts',(-0.0238970429973844,6.90979548741706,
3.64245102870328));
#14333=CARTESIAN_POINT('Ctrl Pts',(0.131586191166419,6.88704931445005,3.8704985271515));
#14334=CARTESIAN_POINT('Ctrl Pts',(0.132036205657411,6.86509836852865,4.13674945418924));
#14335=CARTESIAN_POINT('Ctrl Pts',(-0.0060413687179679,6.84487478558125,
4.33958298894643));
#14336=CARTESIAN_POINT('Ctrl Pts',(-0.204116844890033,6.82641141958407,
4.43475944317313));
#14337=CARTESIAN_POINT('Ctrl Pts',(-0.402473369433673,6.80973569344043,
4.43486896119673));
#14338=CARTESIAN_POINT('Ctrl Pts',(-0.581827228221285,6.79300305116116,
4.34852221416367));
#14339=CARTESIAN_POINT('Ctrl Pts',(-0.706454134874152,6.7762153628094,4.192464816352));
#14340=CARTESIAN_POINT('Ctrl Pts',(-0.751016294559626,6.75937457420164,
3.99715087739011));
#14341=CARTESIAN_POINT('Ctrl Pts',(-0.706447662037028,6.74248271608976,
3.80123388795173));
#14342=CARTESIAN_POINT('Ctrl Pts',(-0.580873534358325,6.72554188917784,
3.64359934962882));
#14343=CARTESIAN_POINT('Ctrl Pts',(-0.398793807750649,6.70855427056295,
3.55588854173989));
#14344=CARTESIAN_POINT('Ctrl Pts',(-0.196213186746174,6.69152210478501,
3.55582569363604));
#14345=CARTESIAN_POINT('Ctrl Pts',(-0.0130963934752721,6.67444770586136,
3.64392728654252));
#14346=CARTESIAN_POINT('Ctrl Pts',(0.113707820363769,6.65733344528682,3.80305624025719));
#14347=CARTESIAN_POINT('Ctrl Pts',(0.164656362590817,6.63827601697293,4.02413741573514));
#14348=CARTESIAN_POINT('Ctrl Pts',(0.0896082709820025,6.61726302509207,
4.2676978223342));
#14349=CARTESIAN_POINT('Ctrl Pts',(-0.110245732077343,6.59619863179822,
4.4270642600818));
#14350=CARTESIAN_POINT('Ctrl Pts',(-0.290838098938005,6.58084997747224,
4.45395573001046));
#14351=CARTESIAN_POINT('Ctrl Pts',(-0.445467117475853,6.56740673782488,
4.43069910759464));
#14352=CARTESIAN_POINT('Ctrl Pts',(-0.589663880409842,6.55395079532829,
4.36131796304211));
#14353=CARTESIAN_POINT('Ctrl Pts',(-0.718225707768932,6.53662851071928,
4.20020661739991));
#14354=CARTESIAN_POINT('Ctrl Pts',(-0.763898158866166,6.51928717897976,
3.99912848715837));
#14355=CARTESIAN_POINT('Ctrl Pts',(-0.710721419612997,6.49903664059857,
3.764202830041));
#14356=CARTESIAN_POINT('Ctrl Pts',(-0.510149997687367,6.47587070043553,
3.56253207697483));
#14357=CARTESIAN_POINT('Ctrl Pts',(-0.227250362890276,6.45268625633124,
3.53107252428385));
#14358=CARTESIAN_POINT('Ctrl Pts',(-0.00982453983942397,6.43239259089565,
3.63631313688574));
#14359=CARTESIAN_POINT('Ctrl Pts',(0.119224416062016,6.414995879623,3.79796488057796));
#14360=CARTESIAN_POINT('Ctrl Pts',(0.161414220224748,6.39904954972701,3.98302626625864));
#14361=CARTESIAN_POINT('Ctrl Pts',(0.132781651753175,6.38455548538367,4.15109736344141));
#14362=CARTESIAN_POINT('Ctrl Pts',(0.058591217696994,6.37151403493753,4.28547086198332));
#14363=CARTESIAN_POINT('Ctrl Pts',(-0.0558362639783319,6.35847699034469,
4.38747481451575));
#14364=CARTESIAN_POINT('Ctrl Pts',(-0.244624220570673,6.34110173177432,
4.46620946091905));
#14365=CARTESIAN_POINT('Ctrl Pts',(-0.509258386493358,6.31939963958705,
4.43663450707748));
#14366=CARTESIAN_POINT('Ctrl Pts',(-0.735030443095589,6.29339375292805,
4.21063569075453));
#14367=CARTESIAN_POINT('Ctrl Pts',(-0.770492148406669,6.2674338232997,3.89395438143295));
#14368=CARTESIAN_POINT('Ctrl Pts',(-0.601210048531917,6.24152902186401,
3.62457992816658));
#14369=CARTESIAN_POINT('Ctrl Pts',(-0.351688619951789,6.21999512440529,
3.53770552245775));
#14370=CARTESIAN_POINT('Ctrl Pts',(-0.152299417857812,6.20280445728418,
3.57207084012085));
#14371=CARTESIAN_POINT('Ctrl Pts',(-0.00495835013055459,6.18850033974624,
3.65330634586973));
#14372=CARTESIAN_POINT('Ctrl Pts',(0.111522803781729,6.17279483671223,3.79940640678234));
#14373=CARTESIAN_POINT('Ctrl Pts',(0.156701474788417,6.15570021231953,3.99770463755195));
#14374=CARTESIAN_POINT('Ctrl Pts',(0.115262604711903,6.14006777305336,4.17897821875209));
#14375=CARTESIAN_POINT('Ctrl Pts',(0.0185932180471106,6.12588811043834,
4.31497113433199));
#14376=CARTESIAN_POINT('Ctrl Pts',(-0.103590553659916,6.11315178814851,
4.4016989608744));
#14377=CARTESIAN_POINT('Ctrl Pts',(-0.247293954733903,6.1004417858412,4.44304193852122));
#14378=CARTESIAN_POINT('Ctrl Pts',(-0.412869049658234,6.08634982725544,
4.43379507168706));
#14379=CARTESIAN_POINT('Ctrl Pts',(-0.578482300908516,6.07088880084204,
4.3539190346138));
#14380=CARTESIAN_POINT('Ctrl Pts',(-0.703246723757797,6.05407432044984,
4.19753682982269));
#14381=CARTESIAN_POINT('Ctrl Pts',(-0.747469580607062,6.03731392465469,
4.00314057125818));
#14382=CARTESIAN_POINT('Ctrl Pts',(-0.703238625925696,6.02060951959296,
3.80940575329504));
#14383=CARTESIAN_POINT('Ctrl Pts',(-0.579634776479789,6.00396293095479,
3.65467865258803));
#14384=CARTESIAN_POINT('Ctrl Pts',(-0.431500759601328,5.99014040360805,
3.58338254073736));
#14385=CARTESIAN_POINT('Ctrl Pts',(-0.303561319206374,5.97911298339926,
3.56906449106088));
#14386=CARTESIAN_POINT('Ctrl Pts',(-0.207808748835976,5.97085791464426,
3.57983145987356));
#14387=CARTESIAN_POINT('Ctrl Pts',(-0.117044922248722,5.96261853714979,
3.6116348383249));
#14388=CARTESIAN_POINT('Ctrl Pts',(-0.00861997369778145,5.95165386736835,
3.67968231581426));
#14389=CARTESIAN_POINT('Ctrl Pts',(0.0926329081004657,5.93798817658918,
3.80681756846826));
#14390=CARTESIAN_POINT('Ctrl Pts',(0.135870644163702,5.92165495155963,3.99626375633351));
#14391=CARTESIAN_POINT('Ctrl Pts',(0.0926387969430078,5.90538860209907,
4.18487776410349));
#14392=CARTESIAN_POINT('Ctrl Pts',(-0.0175125738479973,5.89054016294629,
4.32293582509909));
#14393=CARTESIAN_POINT('Ctrl Pts',(-0.156061008534171,5.87709197920747,
4.39936287338782));
#14394=CARTESIAN_POINT('Ctrl Pts',(-0.296018497756522,5.86502791432804,
4.42315611503599));
#14395=CARTESIAN_POINT('Ctrl Pts',(-0.435406476921251,5.8530035361086,4.39932451423293));
#14396=CARTESIAN_POINT('Ctrl Pts',(-0.600212844195293,5.83702437044493,
4.30861645270809));
#14397=CARTESIAN_POINT('Ctrl Pts',(-0.729945333339283,5.81715142573852,
4.10216892170714));
#14398=CARTESIAN_POINT('Ctrl Pts',(-0.696976009348358,5.7934671926544,3.81306008549607));
#14399=CARTESIAN_POINT('Ctrl Pts',(-0.492652698548329,5.76994854996481,
3.60918617550531));
#14400=CARTESIAN_POINT('Ctrl Pts',(-0.207515825799976,5.74659510021081,
3.57736699868709));
#14401=CARTESIAN_POINT('Ctrl Pts',(-0.00714719245692835,5.72727465695078,
3.70390131122158));
#14402=CARTESIAN_POINT('Ctrl Pts',(0.0800330609517386,5.71189866882786,
3.86253474741929));
#14403=CARTESIAN_POINT('Ctrl Pts',(0.0951821641861108,5.70424160396714,
3.95121652410011));
#14404=CARTESIAN_POINT('Ctrl Pts',(0.0951881709252366,5.70041484319491,
3.99573871784903));
#14405=CARTESIAN_POINT('Origin',(0.1,5.75,4.));
#14406=CARTESIAN_POINT('Origin',(0.1,5.75,4.));
#14407=CARTESIAN_POINT('Origin',(0.1,7.05,4.));
#14408=CARTESIAN_POINT('',(0.,0.,0.));
#14409=CARTESIAN_POINT('Origin',(5.5,5.4,4.));
#14410=CARTESIAN_POINT('',(4.8,5.7,4.));
#14411=CARTESIAN_POINT('Origin',(5.5,5.7,4.));
#14412=CARTESIAN_POINT('',(4.8,5.4,4.));
#14413=CARTESIAN_POINT('',(4.8,5.4,4.));
#14414=CARTESIAN_POINT('Origin',(5.5,5.4,4.));
#14415=CARTESIAN_POINT('Origin',(5.5,5.7,4.));
#14416=CARTESIAN_POINT('Origin',(5.5,5.4,4.));
#14417=CARTESIAN_POINT('',(0.,0.,0.));
#14418=CARTESIAN_POINT('Origin',(5.5,7.1,4.));
#14419=CARTESIAN_POINT('',(4.8,7.4,4.));
#14420=CARTESIAN_POINT('Origin',(5.5,7.4,4.));
#14421=CARTESIAN_POINT('',(4.8,7.1,4.));
#14422=CARTESIAN_POINT('',(4.8,7.1,4.));
#14423=CARTESIAN_POINT('Origin',(5.5,7.1,4.));
#14424=CARTESIAN_POINT('Origin',(5.5,7.4,4.));
#14425=CARTESIAN_POINT('Origin',(5.5,7.1,4.));
#14426=CARTESIAN_POINT('',(0.,0.,0.));
#14427=CARTESIAN_POINT('Ctrl Pts',(5.89999942231746,7.09981632447119,4.00428180053801));
#14428=CARTESIAN_POINT('Ctrl Pts',(5.89999334367971,7.09594376396835,4.04933684813297));
#14429=CARTESIAN_POINT('Ctrl Pts',(5.88465017335476,7.08819405075721,4.13908165517953));
#14430=CARTESIAN_POINT('Ctrl Pts',(5.7964860030169,7.07263331806119,4.29968204261715));
#14431=CARTESIAN_POINT('Ctrl Pts',(5.59351456200701,7.05308119240215,4.4275031391656));
#14432=CARTESIAN_POINT('Ctrl Pts',(5.30510775645105,7.02945158726801,4.39546636939848));
#14433=CARTESIAN_POINT('Ctrl Pts',(5.09844717527872,7.00565845259414,4.18908156433879));
#14434=CARTESIAN_POINT('Ctrl Pts',(5.06491507736497,6.98170283632427,3.89688445847127));
#14435=CARTESIAN_POINT('Ctrl Pts',(5.22229231109316,6.957587725778,3.64598811283775));
#14436=CARTESIAN_POINT('Ctrl Pts',(5.50350105188817,6.93331581944121,3.54720017800962));
#14437=CARTESIAN_POINT('Ctrl Pts',(5.77606730494162,6.90979543600253,3.64243302852389));
#14438=CARTESIAN_POINT('Ctrl Pts',(5.93155863446605,6.88704927881041,3.87048202703801));
#14439=CARTESIAN_POINT('Ctrl Pts',(5.93201459027321,6.86509833940111,4.13672884061229));
#14440=CARTESIAN_POINT('Ctrl Pts',(5.79395734371705,6.84487476341531,4.33956419787309));
#14441=CARTESIAN_POINT('Ctrl Pts',(5.59585169142646,6.82641140225049,4.43472796239094));
#14442=CARTESIAN_POINT('Ctrl Pts',(5.43062330290708,6.81251496798271,4.43483227755276));
#14443=CARTESIAN_POINT('Ctrl Pts',(5.30781628774365,6.8013693608627,4.39175312056372));
#14444=CARTESIAN_POINT('Ctrl Pts',(5.19743069189207,6.79020509173472,4.32251414855249));
#14445=CARTESIAN_POINT('Ctrl Pts',(5.09353798605695,6.77621535562195,4.1924772803632));
#14446=CARTESIAN_POINT('Ctrl Pts',(5.04898925851302,6.75937456735607,3.99715324700454));
#14447=CARTESIAN_POINT('Ctrl Pts',(5.0935413464267,6.74248271039737,3.80123524176677));
#14448=CARTESIAN_POINT('Ctrl Pts',(5.21917592334569,6.72554188446977,3.64363320271165));
#14449=CARTESIAN_POINT('Ctrl Pts',(5.40122000385758,6.70855426693318,3.55590244763416));
#14450=CARTESIAN_POINT('Ctrl Pts',(5.60380955719718,6.6915221019177,3.55584448787041));
#14451=CARTESIAN_POINT('Ctrl Pts',(5.78691645390742,6.67444770371231,3.64394104146688));
#14452=CARTESIAN_POINT('Ctrl Pts',(5.91372041331327,6.65733344366189,3.80307026683985));
#14453=CARTESIAN_POINT('Ctrl Pts',(5.96466327221314,6.63827601600008,4.02414934139344));
#14454=CARTESIAN_POINT('Ctrl Pts',(5.88961383686182,6.61726302422527,4.26770951451258));
#14455=CARTESIAN_POINT('Ctrl Pts',(5.68975602864846,6.59619863118807,4.42707389952551));
#14456=CARTESIAN_POINT('Ctrl Pts',(5.50916223586277,6.58084997697241,4.45396467698472));
#14457=CARTESIAN_POINT('Ctrl Pts',(5.35453310810722,6.56740673736238,4.43070717074375));
#14458=CARTESIAN_POINT('Ctrl Pts',(5.21033393748589,6.55395079494006,4.36132595428699));
#14459=CARTESIAN_POINT('Ctrl Pts',(5.08177516019845,6.53662851034176,4.20021226638331));
#14460=CARTESIAN_POINT('Ctrl Pts',(5.03609211123456,6.51928717867399,3.99913913108666));
#14461=CARTESIAN_POINT('Ctrl Pts',(5.08928582945947,6.49903664031616,3.76419897777231));
#14462=CARTESIAN_POINT('Ctrl Pts',(5.28978283301087,6.47587070029814,3.56256415950519));
#14463=CARTESIAN_POINT('Ctrl Pts',(5.57279015344961,6.4526862562021,3.53101713469425));
#14464=CARTESIAN_POINT('Ctrl Pts',(5.7744501239661,6.4338421384389,3.62890875798563));
#14465=CARTESIAN_POINT('Ctrl Pts',(5.91107614262552,6.41644569471267,3.78134048060785));
#14466=CARTESIAN_POINT('Ctrl Pts',(5.96451577569518,6.40049895608791,3.96616344909838));
#14467=CARTESIAN_POINT('Ctrl Pts',(5.9327299609379,6.3845554854669,4.15104965949736));
#14468=CARTESIAN_POINT('Ctrl Pts',(5.83415684595966,6.36716688464879,4.33040203531341));
#14469=CARTESIAN_POINT('Ctrl Pts',(5.60855787080152,6.3454421500065,4.47243154476512));
#14470=CARTESIAN_POINT('Ctrl Pts',(5.29067075546292,6.31939963984916,4.43654609473001));
#14471=CARTESIAN_POINT('Ctrl Pts',(5.06495666340114,6.29339375333233,4.21070709279472));
#14472=CARTESIAN_POINT('Ctrl Pts',(5.02940089438198,6.26743382198568,3.89407398616837));
#14473=CARTESIAN_POINT('Ctrl Pts',(5.19880065125732,6.24152902171826,3.62471661866899));
#14474=CARTESIAN_POINT('Ctrl Pts',(5.49820781434257,6.21568834443117,3.52014376389726));
#14475=CARTESIAN_POINT('Ctrl Pts',(5.74701061020189,6.19421520170402,3.60728770872527));
#14476=CARTESIAN_POINT('Ctrl Pts',(5.85863359577984,6.17993370216935,3.73296424281348));
#14477=CARTESIAN_POINT('Ctrl Pts',(5.92288006435656,6.16852118154694,3.84896516413552));
#14478=CARTESIAN_POINT('Ctrl Pts',(5.95664235896203,6.15570021350747,3.99755228818456));
#14479=CARTESIAN_POINT('Ctrl Pts',(5.90422907170185,6.13580438066566,4.22863954557107));
#14480=CARTESIAN_POINT('Ctrl Pts',(5.74463079333177,6.1173884553624,4.38823789360272));
#14481=CARTESIAN_POINT('Ctrl Pts',(5.55259803695828,6.10044178794059,4.44287010078724));
#14482=CARTESIAN_POINT('Ctrl Pts',(5.38717753744307,6.08634982964905,4.43381260797737));
#14483=CARTESIAN_POINT('Ctrl Pts',(5.22149962135128,6.07088880373497,4.35387124517548));
#14484=CARTESIAN_POINT('Ctrl Pts',(5.09676922730111,6.0540743240685,4.197519449458));
#14485=CARTESIAN_POINT('Ctrl Pts',(5.0525318165955,6.03731392845979,4.00312051246728));
#14486=CARTESIAN_POINT('Ctrl Pts',(5.09677460214568,6.02060952469266,3.80936725739853));
#14487=CARTESIAN_POINT('Ctrl Pts',(5.22036100773764,6.00396293698029,3.65469518694587));
#14488=CARTESIAN_POINT('Ctrl Pts',(5.39815221757406,5.98737590584214,3.56901265908242));
#14489=CARTESIAN_POINT('Ctrl Pts',(5.56194673621828,5.9736043825902,3.56918712785721));
#14490=CARTESIAN_POINT('Ctrl Pts',(5.6678409475086,5.96399177625527,3.60634259138081));
#14491=CARTESIAN_POINT('Ctrl Pts',(5.72360710674561,5.9585067948969,3.63716464071472));
#14492=CARTESIAN_POINT('Ctrl Pts',(5.80152037634414,5.9502873075744,3.69239994875946));
#14493=CARTESIAN_POINT('Ctrl Pts',(5.89262775771971,5.93798818799799,3.80682412790902));
#14494=CARTESIAN_POINT('Ctrl Pts',(5.93588165070209,5.9216549676263,3.9962737943898));
#14495=CARTESIAN_POINT('Ctrl Pts',(5.89265315890838,5.90538862230925,4.18485446150754));
#14496=CARTESIAN_POINT('Ctrl Pts',(5.78249899819111,5.89054018760752,4.32296861862104));
#14497=CARTESIAN_POINT('Ctrl Pts',(5.64397324912796,5.87709200642215,4.39928196165792));
#14498=CARTESIAN_POINT('Ctrl Pts',(5.45729571883929,5.86100659113963,4.43140768516966));
#14499=CARTESIAN_POINT('Ctrl Pts',(5.22574876053333,5.84099901355926,4.35024097908663));
#14500=CARTESIAN_POINT('Ctrl Pts',(5.0699063365284,5.81715142001874,4.10208650989737));
#14501=CARTESIAN_POINT('Ctrl Pts',(5.10298913581097,5.79346725679344,3.81314318112568));
#14502=CARTESIAN_POINT('Ctrl Pts',(5.30729513304354,5.76994860790156,3.60917536341897));
#14503=CARTESIAN_POINT('Ctrl Pts',(5.59246492988907,5.74659517888843,3.57738640664907));
#14504=CARTESIAN_POINT('Ctrl Pts',(5.79284572265032,5.72727468967069,3.7038989587173));
#14505=CARTESIAN_POINT('Ctrl Pts',(5.8800308145667,5.71189869700794,3.86253471396896));
#14506=CARTESIAN_POINT('Ctrl Pts',(5.8951821641861,5.70424160396714,3.95121652410008));
#14507=CARTESIAN_POINT('Ctrl Pts',(5.89518817092524,5.70041484319491,3.99573871784903));
#14508=CARTESIAN_POINT('Ctrl Pts',(5.88503945743652,7.09981632447119,4.0042797822024));
#14509=CARTESIAN_POINT('Ctrl Pts',(5.88503360188162,7.09608588493208,4.04768133289771));
#14510=CARTESIAN_POINT('Ctrl Pts',(5.87026126699026,7.08862396394419,4.13409876124989));
#14511=CARTESIAN_POINT('Ctrl Pts',(5.78535030584819,7.07363703375696,4.28878882173021));
#14512=CARTESIAN_POINT('Ctrl Pts',(5.58981457160439,7.05480252942765,4.41195005833011));
#14513=CARTESIAN_POINT('Ctrl Pts',(5.31179486198712,7.03202561227573,4.38109726858311));
#14514=CARTESIAN_POINT('Ctrl Pts',(5.1124277587765,7.00907674704486,4.18203908678982));
#14515=CARTESIAN_POINT('Ctrl Pts',(5.08001803350251,6.98595417860409,3.8999761925135));
#14516=CARTESIAN_POINT('Ctrl Pts',(5.23203136694347,6.96266049576345,3.65754564919961));
#14517=CARTESIAN_POINT('Ctrl Pts',(5.50396936937568,6.93919148734548,3.56195831409131));
#14518=CARTESIAN_POINT('Ctrl Pts',(5.76786360761367,6.91642620730754,3.65410210166395));
#14519=CARTESIAN_POINT('Ctrl Pts',(5.91859875131219,6.89438580758112,3.87509306663505));
#14520=CARTESIAN_POINT('Ctrl Pts',(5.91908754056048,6.8730906966479,4.13341261767347));
#14521=CARTESIAN_POINT('Ctrl Pts',(5.78502683264549,6.85345041326714,4.33045812820945));
#14522=CARTESIAN_POINT('Ctrl Pts',(5.59240862903414,6.83550085128541,4.42301346486046));
#14523=CARTESIAN_POINT('Ctrl Pts',(5.43159993473068,6.82197903313836,4.42313220394627));
#14524=CARTESIAN_POINT('Ctrl Pts',(5.31198346558657,6.81112423395334,4.38117622245278));
#14525=CARTESIAN_POINT('Ctrl Pts',(5.20441120090185,6.80024507289894,4.31370604089673));
#14526=CARTESIAN_POINT('Ctrl Pts',(5.10308448889811,6.78660773456135,4.18691472624338));
#14527=CARTESIAN_POINT('Ctrl Pts',(5.05957333477074,6.7701692409416,3.99624133185818));
#14528=CARTESIAN_POINT('Ctrl Pts',(5.10308658178506,6.75366451037247,3.80477816416283));
#14529=CARTESIAN_POINT('Ctrl Pts',(5.22596911064028,6.73709691740872,3.65058727641187));
#14530=CARTESIAN_POINT('Ctrl Pts',(5.40424154502889,6.72046420161793,3.56464409931812));
#14531=CARTESIAN_POINT('Ctrl Pts',(5.60286757635272,6.70376966024345,3.56456110898369));
#14532=CARTESIAN_POINT('Ctrl Pts',(5.78260975317895,6.68701499206993,3.65100600925544));
#14533=CARTESIAN_POINT('Ctrl Pts',(5.90723898021823,6.67020103323329,3.80736557672115));
#14534=CARTESIAN_POINT('Ctrl Pts',(5.95739144160597,6.65145878281361,4.02485643420641));
#14535=CARTESIAN_POINT('Ctrl Pts',(5.88350382080552,6.63075660525971,4.26484435626206));
#14536=CARTESIAN_POINT('Ctrl Pts',(5.68632699032047,6.60997572305765,4.42215495861284));
#14537=CARTESIAN_POINT('Ctrl Pts',(5.50786242867171,6.59481082042869,4.44875398416139));
#14538=CARTESIAN_POINT('Ctrl Pts',(5.35492443239398,6.58151601836513,4.42575382239937));
#14539=CARTESIAN_POINT('Ctrl Pts',(5.21218195064913,6.56819993097658,4.35709671903736));
#14540=CARTESIAN_POINT('Ctrl Pts',(5.08473882673911,6.55103208305566,4.19743115221831));
#14541=CARTESIAN_POINT('Ctrl Pts',(5.03937938103974,6.53382903633989,3.9979075972426));
#14542=CARTESIAN_POINT('Ctrl Pts',(5.09219616215328,6.51371045047149,3.76446604094244));
#14543=CARTESIAN_POINT('Ctrl Pts',(5.29164216583296,6.49066863108082,3.56375987550904));
#14544=CARTESIAN_POINT('Ctrl Pts',(5.57380855674231,6.46755668746403,3.53221661138612));
#14545=CARTESIAN_POINT('Ctrl Pts',(5.77520948735709,6.44874487708301,3.62994883143992));
#14546=CARTESIAN_POINT('Ctrl Pts',(5.9118194085888,6.4313515231649,3.78234207954662));
#14547=CARTESIAN_POINT('Ctrl Pts',(5.96535290798642,6.41539494756269,3.96733324055338));
#14548=CARTESIAN_POINT('Ctrl Pts',(5.93350724448179,6.39941600080786,4.15265573762338));
#14549=CARTESIAN_POINT('Ctrl Pts',(5.83462795102543,6.38197230496921,4.3326009207179));
#14550=CARTESIAN_POINT('Ctrl Pts',(5.60802480207367,6.36015239803693,4.47536066940383));
#14551=CARTESIAN_POINT('Ctrl Pts',(5.28804071704905,6.33394375008401,4.43934003157992));
#14552=CARTESIAN_POINT('Ctrl Pts',(5.0603505371736,6.30772509227727,4.2116637907064));
#14553=CARTESIAN_POINT('Ctrl Pts',(5.02433426469034,6.28150024364713,3.89177497027619));
#14554=CARTESIAN_POINT('Ctrl Pts',(5.19569399285247,6.25529612930055,3.61911293303289));
#14555=CARTESIAN_POINT('Ctrl Pts',(5.49925070212339,6.22909620166617,3.51299220778051));
#14556=CARTESIAN_POINT('Ctrl Pts',(5.75197475889608,6.20729451095337,3.60142940412264));
#14557=CARTESIAN_POINT('Ctrl Pts',(5.86550798533523,6.19277158813603,3.72923955502794));
#14558=CARTESIAN_POINT('Ctrl Pts',(5.93088617148282,6.18115900724412,3.8472804234726));
#14559=CARTESIAN_POINT('Ctrl Pts',(5.96528306606778,6.16810503068496,3.99858218016166));
#14560=CARTESIAN_POINT('Ctrl Pts',(5.91188622152517,6.14782425772989,4.23416182125941));
#14561=CARTESIAN_POINT('Ctrl Pts',(5.7490193624655,6.12903078679408,4.39711001697646));
#14562=CARTESIAN_POINT('Ctrl Pts',(5.55277074738954,6.11171437387845,4.45295636322444));
#14563=CARTESIAN_POINT('Ctrl Pts',(5.38358725567555,6.09730363521905,4.44370269520848));
#14564=CARTESIAN_POINT('Ctrl Pts',(5.21398497489651,6.08147921618268,4.3618860003188));
#14565=CARTESIAN_POINT('Ctrl Pts',(5.08616324600684,6.06425310299918,4.20169628716414));
#14566=CARTESIAN_POINT('Ctrl Pts',(5.04077402087937,6.04706393365499,4.00231532025332));
#14567=CARTESIAN_POINT('Ctrl Pts',(5.08617032093218,6.02991837734054,3.80341237994541));
#14568=CARTESIAN_POINT('Ctrl Pts',(5.21314140461402,6.01281654577742,3.64447952839659));
#14569=CARTESIAN_POINT('Ctrl Pts',(5.39596558147649,5.99576114159946,3.55635140588749));
#14570=CARTESIAN_POINT('Ctrl Pts',(5.56454843416681,5.98158811350942,3.55651828149823));
#14571=CARTESIAN_POINT('Ctrl Pts',(5.67360413989068,5.97168893571421,3.59478043709277));
#14572=CARTESIAN_POINT('Ctrl Pts',(5.73105166386915,5.96603869488852,3.62653169595776));
#14573=CARTESIAN_POINT('Ctrl Pts',(5.8113292722746,5.95756999758158,3.68344222347348));
#14574=CARTESIAN_POINT('Ctrl Pts',(5.90525200105339,5.94489303633764,3.80138469729133));
#14575=CARTESIAN_POINT('Ctrl Pts',(5.9498859624265,5.92804546902486,3.99680740667185));
#14576=CARTESIAN_POINT('Ctrl Pts',(5.90527406073601,5.91125567170158,4.19147367065731));
#14577=CARTESIAN_POINT('Ctrl Pts',(5.79150254559316,5.89591895994826,4.33414205895609));
#14578=CARTESIAN_POINT('Ctrl Pts',(5.64834101429215,5.88202102372911,4.4130140624278));
#14579=CARTESIAN_POINT('Ctrl Pts',(5.4553346472487,5.86539043683629,4.44623569719961));
#14580=CARTESIAN_POINT('Ctrl Pts',(5.21578000821573,5.84469228785158,4.36229253299229));
#14581=CARTESIAN_POINT('Ctrl Pts',(5.05441367332187,5.82000362720346,4.10540136247045));
#14582=CARTESIAN_POINT('Ctrl Pts',(5.08866429485251,5.79546931039049,3.80607791306765));
#14583=CARTESIAN_POINT('Ctrl Pts',(5.30040509492993,5.77109351117434,3.59466769610795));
#14584=CARTESIAN_POINT('Ctrl Pts',(5.59608563803559,5.74687955036343,3.56169371934204));
#14585=CARTESIAN_POINT('Ctrl Pts',(5.80392030130352,5.72684060107471,3.69290766840958));
#14586=CARTESIAN_POINT('Ctrl Pts',(5.89435424813677,5.71089217884313,3.85744883447212));
#14587=CARTESIAN_POINT('Ctrl Pts',(5.91007247017572,5.70294882509164,3.94944546934017));
#14588=CARTESIAN_POINT('Ctrl Pts',(5.91007869895502,5.69898060743533,3.99561343380099));
#14589=CARTESIAN_POINT('Ctrl Pts',(5.85520827475736,7.08553591511819,4.00304833122987));
#14590=CARTESIAN_POINT('Ctrl Pts',(5.85520286590809,7.08209006146883,4.04313888631962));
#14591=CARTESIAN_POINT('Ctrl Pts',(5.84156747486463,7.07520486942886,4.12287606165967));
#14592=CARTESIAN_POINT('Ctrl Pts',(5.76326212603904,7.06138551553941,4.26551030037515));
#14593=CARTESIAN_POINT('Ctrl Pts',(5.58313571416996,7.04403789214147,4.37890493291776));
#14594=CARTESIAN_POINT('Ctrl Pts',(5.32733643620847,7.02308074340475,4.35047304239883));
#14595=CARTESIAN_POINT('Ctrl Pts',(5.14406551156473,7.00198204308889,4.16743848880527));
#14596=CARTESIAN_POINT('Ctrl Pts',(5.11430140308165,6.98073307206542,3.90823568037324));
#14597=CARTESIAN_POINT('Ctrl Pts',(5.2539756967838,6.9593299476571,3.68549505746316));
#14598=CARTESIAN_POINT('Ctrl Pts',(5.50385557975491,6.93776292440614,3.59765170680461));
#14599=CARTESIAN_POINT('Ctrl Pts',(5.746454002493,6.91683348560458,3.68233751904534));
#14600=CARTESIAN_POINT('Ctrl Pts',(5.88513081194609,6.89655721527044,3.8856066901103));
#14601=CARTESIAN_POINT('Ctrl Pts',(5.88561108039455,6.87695122617721,4.12342024789602));
#14602=CARTESIAN_POINT('Ctrl Pts',(5.7620912805646,6.85884906967209,4.30503249532845));
#14603=CARTESIAN_POINT('Ctrl Pts',(5.58439221890232,6.84228705858853,4.39044285766885));
#14604=CARTESIAN_POINT('Ctrl Pts',(5.43587731018536,6.82979711795253,4.39056857002489));
#14605=CARTESIAN_POINT('Ctrl Pts',(5.32531224002107,6.81976316059046,4.35179163381183));
#14606=CARTESIAN_POINT('Ctrl Pts',(5.22582219123238,6.80970122556429,4.28939485292107));
#14607=CARTESIAN_POINT('Ctrl Pts',(5.13200246986364,6.79707273454254,4.17202717151191));
#14608=CARTESIAN_POINT('Ctrl Pts',(5.09164094749547,6.78183341704652,3.99528331468449));
#14609=CARTESIAN_POINT('Ctrl Pts',(5.13200751743207,6.7665098094977,3.81754003421871));
#14610=CARTESIAN_POINT('Ctrl Pts',(5.24623575349236,6.75110199174121,3.67415956298011));
#14611=CARTESIAN_POINT('Ctrl Pts',(5.41224144571201,6.73560920651841,3.59409517730086));
#14612=CARTESIAN_POINT('Ctrl Pts',(5.59753307127925,6.72003176914412,3.59398376812156));
#14613=CARTESIAN_POINT('Ctrl Pts',(5.76552583542977,6.7043697251995,3.67473816518997));
#14614=CARTESIAN_POINT('Ctrl Pts',(5.88224637668914,6.68862335676344,3.82111570717619));
#14615=CARTESIAN_POINT('Ctrl Pts',(5.92933877872348,6.67103426452799,4.02514024338844));
#14616=CARTESIAN_POINT('Ctrl Pts',(5.85995562430613,6.65156702212541,4.25083041727868));
#14617=CARTESIAN_POINT('Ctrl Pts',(5.67407637808894,6.63196546184507,4.39925506328189));
#14618=CARTESIAN_POINT('Ctrl Pts',(5.50535216060145,6.61762539342909,4.42444600623728));
#14619=CARTESIAN_POINT('Ctrl Pts',(5.3605465743758,6.60503616153032,4.40267199067841));
#14620=CARTESIAN_POINT('Ctrl Pts',(5.22516696857318,6.59240538591147,4.33759897336023));
#14621=CARTESIAN_POINT('Ctrl Pts',(5.10399727465634,6.57608706132853,4.18587447130434));
#14622=CARTESIAN_POINT('Ctrl Pts',(5.06072881807943,6.55969079980481,3.9957755594979));
#14623=CARTESIAN_POINT('Ctrl Pts',(5.11111408899349,6.54047310824596,3.77281018900098));
#14624=CARTESIAN_POINT('Ctrl Pts',(5.30208506774464,6.51838444294906,3.58039325945438));
#14625=CARTESIAN_POINT('Ctrl Pts',(5.57344463256731,6.49615180944088,3.54987434760595));
#14626=CARTESIAN_POINT('Ctrl Pts',(5.76781931146614,6.47799290930932,3.64412456683428));
#14627=CARTESIAN_POINT('Ctrl Pts',(5.89995287193516,6.46117266087352,3.79146891932382));
#14628=CARTESIAN_POINT('Ctrl Pts',(5.95194793315776,6.44569200784306,3.97083844037072));
#14629=CARTESIAN_POINT('Ctrl Pts',(5.92101524437169,6.43015394352054,4.15103610674214));
#14630=CARTESIAN_POINT('Ctrl Pts',(5.82471537837473,6.41315680171824,4.32636138876989));
#14631=CARTESIAN_POINT('Ctrl Pts',(5.60334919178702,6.39182442975737,4.46603253787654));
#14632=CARTESIAN_POINT('Ctrl Pts',(5.28930632440049,6.36609845573924,4.43091101628552));
#14633=CARTESIAN_POINT('Ctrl Pts',(5.06476647708227,6.34025240232702,4.20670542372654));
#14634=CARTESIAN_POINT('Ctrl Pts',(5.02889907069948,6.3142971139968,3.89017648193371));
#14635=CARTESIAN_POINT('Ctrl Pts',(5.19901272516604,6.28823592961183,3.61906735374071));
#14636=CARTESIAN_POINT('Ctrl Pts',(5.50187330256082,6.26208782732235,3.51294889123812));
#14637=CARTESIAN_POINT('Ctrl Pts',(5.75522864687994,6.24022603278353,3.60140445329964));
#14638=CARTESIAN_POINT('Ctrl Pts',(5.8694004766967,6.22562326388648,3.72988152914194));
#14639=CARTESIAN_POINT('Ctrl Pts',(5.93521917425819,6.21393138166647,3.84871410099053));
#14640=CARTESIAN_POINT('Ctrl Pts',(5.9699545000092,6.2007640404577,4.00129391329599));
#14641=CARTESIAN_POINT('Ctrl Pts',(5.91603232645555,6.18025175472434,4.23954868417462));
#14642=CARTESIAN_POINT('Ctrl Pts',(5.75085163785764,6.16117154945629,4.40502717202795));
#14643=CARTESIAN_POINT('Ctrl Pts',(5.55107490688255,6.1435399111569,4.46192298098248));
#14644=CARTESIAN_POINT('Ctrl Pts',(5.37850386197236,6.12883720723606,4.45250910417445));
#14645=CARTESIAN_POINT('Ctrl Pts',(5.20506062246286,6.11265360212113,4.36891210542381));
#14646=CARTESIAN_POINT('Ctrl Pts',(5.07397022510475,6.09498817543275,4.20471986456681));
#14647=CARTESIAN_POINT('Ctrl Pts',(5.02724887723126,6.07731784476976,3.99979245739442));
#14648=CARTESIAN_POINT('Ctrl Pts',(5.07398000181797,6.05964215966279,3.79478075744986));
#14649=CARTESIAN_POINT('Ctrl Pts',(5.20512899117882,6.04196680287455,3.63051306675947));
#14650=CARTESIAN_POINT('Ctrl Pts',(5.39449791013073,6.02429430077605,3.53916197577409));
#14651=CARTESIAN_POINT('Ctrl Pts',(5.56957457418985,6.00957349714106,3.53928300415917));
#14652=CARTESIAN_POINT('Ctrl Pts',(5.68304311953453,5.99927347455427,3.57908441449588));
#14653=CARTESIAN_POINT('Ctrl Pts',(5.74286750570382,5.99338929587818,3.61214779557074));
#14654=CARTESIAN_POINT('Ctrl Pts',(5.82651752458846,5.98456439340875,3.67144751047707));
#14655=CARTESIAN_POINT('Ctrl Pts',(5.92457367352351,5.97133175061034,3.79451182749295));
#14656=CARTESIAN_POINT('Ctrl Pts',(5.97131861714195,5.95370439896441,3.99893579046224));
#14657=CARTESIAN_POINT('Ctrl Pts',(5.92459901326296,5.9360961851512,4.20307083437987));
#14658=CARTESIAN_POINT('Ctrl Pts',(5.80507236487523,5.91997636067228,4.35303796134367));
#14659=CARTESIAN_POINT('Ctrl Pts',(5.65434040611686,5.90534114871628,4.43611034923164));
#14660=CARTESIAN_POINT('Ctrl Pts',(5.45079337565466,5.88779962963185,4.47118188652743));
#14661=CARTESIAN_POINT('Ctrl Pts',(5.19748767042105,5.86591465359703,4.38257023322066));
#14662=CARTESIAN_POINT('Ctrl Pts',(5.0262253355364,5.83973026581737,4.1102456118929));
#14663=CARTESIAN_POINT('Ctrl Pts',(5.06249311301707,5.81363157422294,3.79188150756157));
#14664=CARTESIAN_POINT('Ctrl Pts',(5.28820296732657,5.78763167671582,3.56632359857709));
#14665=CARTESIAN_POINT('Ctrl Pts',(5.60433171174338,5.76173879777121,3.53092676719688));
#14666=CARTESIAN_POINT('Ctrl Pts',(5.8271423468097,5.74025670777543,3.67148617104396));
#14667=CARTESIAN_POINT('Ctrl Pts',(5.92424341235541,5.72313628975845,3.84810607771893));
#14668=CARTESIAN_POINT('Ctrl Pts',(5.94114425819813,5.71459769800728,3.94698841008634));
#14669=CARTESIAN_POINT('Ctrl Pts',(5.94115094957305,5.7103347709078,3.99658515196739));
#14670=CARTESIAN_POINT('Ctrl Pts',(5.8442633579502,7.03733205433023,3.99890364805841));
#14671=CARTESIAN_POINT('Ctrl Pts',(5.8442581197547,7.033994920285,4.03772931214518));
#14672=CARTESIAN_POINT('Ctrl Pts',(5.83104037018746,7.02733254813469,4.11486923947922));
#14673=CARTESIAN_POINT('Ctrl Pts',(5.75552618055734,7.01401654539893,4.25226823033117));
#14674=CARTESIAN_POINT('Ctrl Pts',(5.58280384378936,6.99739080062923,4.36069793188289));
#14675=CARTESIAN_POINT('Ctrl Pts',(5.33962002405483,6.97746235757696,4.33335540787856));
#14676=CARTESIAN_POINT('Ctrl Pts',(5.16682890132043,6.95754317780304,4.16039369672885));
#14677=CARTESIAN_POINT('Ctrl Pts',(5.13920853014916,6.93762223295465,3.91740209304229));
#14678=CARTESIAN_POINT('Ctrl Pts',(5.26947333563793,6.91768645343595,3.71016409897338));
#14679=CARTESIAN_POINT('Ctrl Pts',(5.50072401296219,6.89772870913039,3.62914290710299));
#14680=CARTESIAN_POINT('Ctrl Pts',(5.72372388246367,6.87847647854881,3.70723339336683));
#14681=CARTESIAN_POINT('Ctrl Pts',(5.85042194476176,6.85992603432529,3.89324231795015));
#14682=CARTESIAN_POINT('Ctrl Pts',(5.85070963937428,6.84207613283086,4.10972981319966));
#14683=CARTESIAN_POINT('Ctrl Pts',(5.73865422141122,6.82566665538221,4.27425669236962));
#14684=CARTESIAN_POINT('Ctrl Pts',(5.57815357745207,6.810706867649,4.35133307049917));
#14685=CARTESIAN_POINT('Ctrl Pts',(5.44441328362009,6.79945730366432,4.35140747521201));
#14686=CARTESIAN_POINT('Ctrl Pts',(5.34505646175606,6.79043938302152,4.31655337572742));
#14687=CARTESIAN_POINT('Ctrl Pts',(5.25576788953666,6.78140860275172,4.26054606594844));
#14688=CARTESIAN_POINT('Ctrl Pts',(5.1717433274605,6.77009209107834,4.15537468511295));
#14689=CARTESIAN_POINT('Ctrl Pts',(5.13570651291062,6.75647039032151,3.99739589300255));
#14690=CARTESIAN_POINT('Ctrl Pts',(5.17174572160623,6.74280160059864,3.83886918353745));
#14691=CARTESIAN_POINT('Ctrl Pts',(5.27346273046517,6.72908234649353,3.71124281622253));
#14692=CARTESIAN_POINT('Ctrl Pts',(5.42101179131082,6.71531148066912,3.6401110882049));
#14693=CARTESIAN_POINT('Ctrl Pts',(5.58544422096062,6.70148584866942,3.64003580689892));
#14694=CARTESIAN_POINT('Ctrl Pts',(5.73432346049268,6.68760313547377,3.71162565604183));
#14695=CARTESIAN_POINT('Ctrl Pts',(5.83764552929192,6.67366116797505,3.84122520535718));
#14696=CARTESIAN_POINT('Ctrl Pts',(5.87928444298638,6.658100912098,4.02169607449061));
#14697=CARTESIAN_POINT('Ctrl Pts',(5.81794296845177,6.64089543827006,4.22115320816706));
#14698=CARTESIAN_POINT('Ctrl Pts',(5.6537487144978,6.62358017931584,4.35224741413031));
#14699=CARTESIAN_POINT('Ctrl Pts',(5.50474573233506,6.61091566681907,4.37449449482154));
#14700=CARTESIAN_POINT('Ctrl Pts',(5.3768646872216,6.59979765360415,4.35526579110611));
#14701=CARTESIAN_POINT('Ctrl Pts',(5.25729954874086,6.58864209789496,4.29779828729648));
#14702=CARTESIAN_POINT('Ctrl Pts',(5.15025342040901,6.5742265315835,4.16377038217943));
#14703=CARTESIAN_POINT('Ctrl Pts',(5.11200030526049,6.55973534828414,3.99576364180229));
#14704=CARTESIAN_POINT('Ctrl Pts',(5.15654185679476,6.54274034280373,3.79858438441201));
#14705=CARTESIAN_POINT('Ctrl Pts',(5.32554784904026,6.52318707054893,3.62821328392619));
#14706=CARTESIAN_POINT('Ctrl Pts',(5.56613353860405,6.50347523010832,3.60107938902761));
#14707=CARTESIAN_POINT('Ctrl Pts',(5.73877029295882,6.48734943548394,3.68475125508372));
#14708=CARTESIAN_POINT('Ctrl Pts',(5.85627571304628,6.47239252636156,3.81575918380156));
#14709=CARTESIAN_POINT('Ctrl Pts',(5.90263031720046,6.45860635937458,3.97548974074165));
#14710=CARTESIAN_POINT('Ctrl Pts',(5.87505167436944,6.44474372928567,4.13626778107872));
#14711=CARTESIAN_POINT('Ctrl Pts',(5.78903514141083,6.42955803390157,4.29291835106576));
#14712=CARTESIAN_POINT('Ctrl Pts',(5.59088448553645,6.41045798350198,4.41808744129809));
#14713=CARTESIAN_POINT('Ctrl Pts',(5.30873518287549,6.38734750124527,4.38670311299745));
#14714=CARTESIAN_POINT('Ctrl Pts',(5.10615471140587,6.36404684857898,4.18468451257222));
#14715=CARTESIAN_POINT('Ctrl Pts',(5.07349898841052,6.34055522359989,3.8982098092804));
#14716=CARTESIAN_POINT('Ctrl Pts',(5.22791505782553,6.31687679944705,3.65170107095422));
#14717=CARTESIAN_POINT('Ctrl Pts',(5.50431592493739,6.29300768975538,3.55461983394832));
#14718=CARTESIAN_POINT('Ctrl Pts',(5.73671787489177,6.27296418176745,3.6355503842994));
#14719=CARTESIAN_POINT('Ctrl Pts',(5.84183688606317,6.25952452604128,3.75378707156832));
#14720=CARTESIAN_POINT('Ctrl Pts',(5.90252063540586,6.24874582138889,3.86334104486593));
#14721=CARTESIAN_POINT('Ctrl Pts',(5.93466081634591,6.23658242737163,4.00429106496237));
#14722=CARTESIAN_POINT('Ctrl Pts',(5.88477257211492,6.21756897840495,4.22516592599398));
#14723=CARTESIAN_POINT('Ctrl Pts',(5.73112374226898,6.19980983242131,4.37935499119927));
#14724=CARTESIAN_POINT('Ctrl Pts',(5.54437866031431,6.18333055162171,4.43259622705531));
#14725=CARTESIAN_POINT('Ctrl Pts',(5.38261999067874,6.16955106486449,4.42380810286847));
#14726=CARTESIAN_POINT('Ctrl Pts',(5.21948440418905,6.15433461785036,4.34526151688322));
#14727=CARTESIAN_POINT('Ctrl Pts',(5.09567527200945,6.13766356859339,4.19033418142023));
#14728=CARTESIAN_POINT('Ctrl Pts',(5.05132292060661,6.120920804985,3.99616808757238));
#14729=CARTESIAN_POINT('Ctrl Pts',(5.09568013075446,6.10411152452373,3.80114024004156));
#14730=CARTESIAN_POINT('Ctrl Pts',(5.2208564304236,6.08723548924311,3.64421655461967));
#14731=CARTESIAN_POINT('Ctrl Pts',(5.40236843774688,6.07029554676657,3.55655082292256));
#14732=CARTESIAN_POINT('Ctrl Pts',(5.57090761649076,6.05612632794669,3.55659431162632));
#14733=CARTESIAN_POINT('Ctrl Pts',(5.68047831247714,6.04618144828711,3.59501288603736));
#14734=CARTESIAN_POINT('Ctrl Pts',(5.7383337836807,6.04049119521234,3.62698653839934));
#14735=CARTESIAN_POINT('Ctrl Pts',(5.8193132044321,6.03194870990487,3.68438770351889));
#14736=CARTESIAN_POINT('Ctrl Pts',(5.91452854847537,6.0191093147926,3.80377513400947));
#14737=CARTESIAN_POINT('Ctrl Pts',(5.96017726931528,6.00193511332281,4.00295549686061));
#14738=CARTESIAN_POINT('Ctrl Pts',(5.91454763656368,5.98470857921717,4.2027269727812));
#14739=CARTESIAN_POINT('Ctrl Pts',(5.79716877045588,5.96887147306035,4.35014107428084));
#14740=CARTESIAN_POINT('Ctrl Pts',(5.64852424861931,5.95443918265348,4.43210799719531));
#14741=CARTESIAN_POINT('Ctrl Pts',(5.44716731617039,5.93708678955292,4.46686180108763));
#14742=CARTESIAN_POINT('Ctrl Pts',(5.19528800450862,5.91533634052886,4.37903445531321));
#14743=CARTESIAN_POINT('Ctrl Pts',(5.02367424394978,5.88914912040216,4.10682213449717));
#14744=CARTESIAN_POINT('Ctrl Pts',(5.05983407646609,5.86288698339694,3.78630359033442));
#14745=CARTESIAN_POINT('Ctrl Pts',(5.28822019826199,5.83655644865667,3.55758071132317));
#14746=CARTESIAN_POINT('Ctrl Pts',(5.61042287602758,5.81016939852405,3.52114893229972));
#14747=CARTESIAN_POINT('Ctrl Pts',(5.83908979198061,5.78814211888601,3.66511277419047));
#14748=CARTESIAN_POINT('Ctrl Pts',(5.93920546082742,5.77050202961558,3.8470873725861));
#14749=CARTESIAN_POINT('Ctrl Pts',(5.95669478049843,5.76167432127745,3.94932370527045));
#14750=CARTESIAN_POINT('Ctrl Pts',(5.95670170074323,5.75726558623602,4.00061683995683));
#14751=CARTESIAN_POINT('Ctrl Pts',(5.87514548417672,6.99854044864851,3.99557360787966));
#14752=CARTESIAN_POINT('Ctrl Pts',(5.87513978765661,6.99491132651841,4.03779638791872));
#14753=CARTESIAN_POINT('Ctrl Pts',(5.86075022359954,6.98766329031147,4.12172125899622));
#14754=CARTESIAN_POINT('Ctrl Pts',(5.77883107645889,6.97322759641233,4.27068148293984));
#14755=CARTESIAN_POINT('Ctrl Pts',(5.59230633485985,6.95528685852212,4.38753321295925));
#14756=CARTESIAN_POINT('Ctrl Pts',(5.33155020564179,6.93391865832403,4.35791618403263));
#14757=CARTESIAN_POINT('Ctrl Pts',(5.14773246729608,6.91270540416619,4.17347705756876));
#14758=CARTESIAN_POINT('Ctrl Pts',(5.11883580759173,6.89164103056227,3.9164440087751));
#14759=CARTESIAN_POINT('Ctrl Pts',(5.25588116695966,6.87071957668565,3.6990566497247));
#14760=CARTESIAN_POINT('Ctrl Pts',(5.49694403853312,6.84993083868618,3.6149532499762));
#14761=CARTESIAN_POINT('Ctrl Pts',(5.72739217434572,6.83003349550605,3.69599197049964));
#14762=CARTESIAN_POINT('Ctrl Pts',(5.85719964701457,6.81100327064808,3.88700464630704));
#14763=CARTESIAN_POINT('Ctrl Pts',(5.85726081296606,6.79281909841024,4.10758802917809));
#14764=CARTESIAN_POINT('Ctrl Pts',(5.74373291807669,6.77622423972196,4.27389444303247));
#14765=CARTESIAN_POINT('Ctrl Pts',(5.58236852338651,6.76119137058875,4.35125834030399));
#14766=CARTESIAN_POINT('Ctrl Pts',(5.44867419960033,6.74994884661536,4.35125385557247));
#14767=CARTESIAN_POINT('Ctrl Pts',(5.34976030800238,6.74097144095651,4.31653614511533));
#14768=CARTESIAN_POINT('Ctrl Pts',(5.26110773818199,6.73200480430205,4.26090950185114));
#14769=CARTESIAN_POINT('Ctrl Pts',(5.17808610936031,6.72081958457785,4.15686365468362));
#14770=CARTESIAN_POINT('Ctrl Pts',(5.1427384642525,6.70742370332015,4.00146629817937));
#14771=CARTESIAN_POINT('Ctrl Pts',(5.17808628986628,6.69405440549435,3.84640454479009));
#14772=CARTESIAN_POINT('Ctrl Pts',(5.27713337356397,6.68070956969354,3.72228233330786));
#14773=CARTESIAN_POINT('Ctrl Pts',(5.41998780176605,6.66738391686113,3.6535162350639));
#14774=CARTESIAN_POINT('Ctrl Pts',(5.57831764719913,6.65407511732755,3.65353579167895));
#14775=CARTESIAN_POINT('Ctrl Pts',(5.72089719398017,6.64077986955346,3.72219848416115));
#14776=CARTESIAN_POINT('Ctrl Pts',(5.81930953143935,6.62749439614206,3.84577722805825));
#14777=CARTESIAN_POINT('Ctrl Pts',(5.85870394850306,6.61274185884821,4.01697267297566));
#14778=CARTESIAN_POINT('Ctrl Pts',(5.80067105304151,6.59651509694839,4.20503754829806));
#14779=CARTESIAN_POINT('Ctrl Pts',(5.64666780825017,6.58028993315573,4.32776333798744));
#14780=CARTESIAN_POINT('Ctrl Pts',(5.50774076906622,6.56848394985099,4.34843470371925));
#14781=CARTESIAN_POINT('Ctrl Pts',(5.38885142963878,6.55814860077465,4.33055181655375));
#14782=CARTESIAN_POINT('Ctrl Pts',(5.27804026744975,6.54780951370302,4.2772266172093));
#14783=CARTESIAN_POINT('Ctrl Pts',(5.17927293647025,6.53450161770272,4.15344678062057));
#14784=CARTESIAN_POINT('Ctrl Pts',(5.14416812305239,6.52118046944049,3.99895936753469));
#14785=CARTESIAN_POINT('Ctrl Pts',(5.1850453990095,6.50561478324366,3.81835726355173));
#14786=CARTESIAN_POINT('Ctrl Pts',(5.339284997864,6.48779307370435,3.66315400412196));
#14787=CARTESIAN_POINT('Ctrl Pts',(5.55754831918104,6.46991368775191,3.63872503876236));
#14788=CARTESIAN_POINT('Ctrl Pts',(5.71350848036609,6.45534555587482,3.71438173891507));
#14789=CARTESIAN_POINT('Ctrl Pts',(5.81940093081938,6.44186425747974,3.83248890666509));
#14790=CARTESIAN_POINT('Ctrl Pts',(5.86099636209716,6.42947631893566,3.97607363283317));
#14791=CARTESIAN_POINT('Ctrl Pts',(5.83624924861445,6.41704875670862,4.12020838390855));
#14792=CARTESIAN_POINT('Ctrl Pts',(5.75924576580022,6.40345957109736,4.26039065665031));
#14793=CARTESIAN_POINT('Ctrl Pts',(5.58230732141824,6.38641243046477,4.37202924255808));
#14794=CARTESIAN_POINT('Ctrl Pts',(5.33119627254454,6.36584482021927,4.34397642119019));
#14795=CARTESIAN_POINT('Ctrl Pts',(5.15140636995601,6.34515949086949,4.16454562210437));
#14796=CARTESIAN_POINT('Ctrl Pts',(5.12254982607975,6.32434519787953,3.91070033361363));
#14797=CARTESIAN_POINT('Ctrl Pts',(5.25920873518247,6.30340142939672,3.6926602572414));
#14798=CARTESIAN_POINT('Ctrl Pts',(5.50347393537872,6.28230883810381,3.60690759285009));
#14799=CARTESIAN_POINT('Ctrl Pts',(5.70869616727121,6.26461043075207,3.67839455761512));
#14800=CARTESIAN_POINT('Ctrl Pts',(5.80150749996396,6.2527445027482,3.78278841553677));
#14801=CARTESIAN_POINT('Ctrl Pts',(5.8550859977429,6.24322788838423,3.87951569410302));
#14802=CARTESIAN_POINT('Ctrl Pts',(5.88346434910103,6.23248866320778,4.00396460760673));
#14803=CARTESIAN_POINT('Ctrl Pts',(5.83941409539019,6.21569758858433,4.19902206859976));
#14804=CARTESIAN_POINT('Ctrl Pts',(5.70367326626789,6.20000650214883,4.33527098884019));
#14805=CARTESIAN_POINT('Ctrl Pts',(5.53855228655731,6.18543517970738,4.38235651612384));
#14806=CARTESIAN_POINT('Ctrl Pts',(5.39543801792977,6.17324367379672,4.37458667586454));
#14807=CARTESIAN_POINT('Ctrl Pts',(5.25098024432611,6.15976998349194,4.30505194274034));
#14808=CARTESIAN_POINT('Ctrl Pts',(5.14121655731439,6.14499160555445,4.16773264727778));
#14809=CARTESIAN_POINT('Ctrl Pts',(5.10182587914745,6.13013154458964,3.99540643427926));
#14810=CARTESIAN_POINT('Ctrl Pts',(5.14122514831917,6.11519028373789,3.8220564397272));
#14811=CARTESIAN_POINT('Ctrl Pts',(5.25263588248017,6.10016628060021,3.68233820392778));
#14812=CARTESIAN_POINT('Ctrl Pts',(5.41448657988468,6.08505886588137,3.60412985666001));
#14813=CARTESIAN_POINT('Ctrl Pts',(5.56506704731687,6.07239919129658,3.60413578617919));
#14814=CARTESIAN_POINT('Ctrl Pts',(5.66311283101293,6.06350038653797,3.63850704060478));
#14815=CARTESIAN_POINT('Ctrl Pts',(5.7149221186375,6.05840477958295,3.66713842572877));
#14816=CARTESIAN_POINT('Ctrl Pts',(5.78747702938897,6.05075080923013,3.7185669337241));
#14817=CARTESIAN_POINT('Ctrl Pts',(5.87293025946013,6.03923050065618,3.82566146039982));
#14818=CARTESIAN_POINT('Ctrl Pts',(5.91402507704787,6.02378513403553,4.00476477146208));
#14819=CARTESIAN_POINT('Ctrl Pts',(5.87294369145138,6.00825508165675,4.18486099195512));
#14820=CARTESIAN_POINT('Ctrl Pts',(5.76690353827561,5.99394133612039,4.31811566915106));
#14821=CARTESIAN_POINT('Ctrl Pts',(5.63226512122908,5.98086723592559,4.39238906025841));
#14822=CARTESIAN_POINT('Ctrl Pts',(5.44950474947794,5.96511502927026,4.42397005765718));
#14823=CARTESIAN_POINT('Ctrl Pts',(5.22008211053465,5.94530667428613,4.34415650242552));
#14824=CARTESIAN_POINT('Ctrl Pts',(5.06291182507567,5.92134913814384,4.09528547532897));
#14825=CARTESIAN_POINT('Ctrl Pts',(5.09590900327192,5.89720669469332,3.80066624542902));
#14826=CARTESIAN_POINT('Ctrl Pts',(5.30668586808294,5.87288210191658,3.58923668118618));
#14827=CARTESIAN_POINT('Ctrl Pts',(5.60579413240307,5.84838086936144,3.55513713761874));
#14828=CARTESIAN_POINT('Ctrl Pts',(5.81936747109835,5.82781552400804,3.68933059315267));
#14829=CARTESIAN_POINT('Ctrl Pts',(5.91324358998992,5.81128381242343,3.85984598368901));
#14830=CARTESIAN_POINT('Ctrl Pts',(5.92970378689351,5.80298590584205,3.95593351696052));
#14831=CARTESIAN_POINT('Ctrl Pts',(5.92971029794461,5.79883785906193,4.00419369140481));
#14832=CARTESIAN_POINT('Ctrl Pts',(5.92479734822298,6.99869271407564,3.99559339418157));
#14833=CARTESIAN_POINT('Ctrl Pts',(5.92479090997151,6.99459105192559,4.04331390965279));
#14834=CARTESIAN_POINT('Ctrl Pts',(5.90850975380561,6.98638756199577,4.1382994503635));
#14835=CARTESIAN_POINT('Ctrl Pts',(5.8157856671956,6.97004679073908,4.30691427794729));
#14836=CARTESIAN_POINT('Ctrl Pts',(5.60456312519679,6.94972761837475,4.43926282438681));
#14837=CARTESIAN_POINT('Ctrl Pts',(5.30924514470025,6.92552625657262,4.40571412404912));
#14838=CARTESIAN_POINT('Ctrl Pts',(5.10115155224644,6.90150776708021,4.19688142095042));
#14839=CARTESIAN_POINT('Ctrl Pts',(5.06851049643939,6.87767566403273,3.90609185048507));
#14840=CARTESIAN_POINT('Ctrl Pts',(5.22342892068834,6.85403159761471,3.66049532779896));
#14841=CARTESIAN_POINT('Ctrl Pts',(5.49540131761851,6.8305770702376,3.56571109549459));
#14842=CARTESIAN_POINT('Ctrl Pts',(5.75478373950727,6.80817442310058,3.65704418598113));
#14843=CARTESIAN_POINT('Ctrl Pts',(5.90047506910969,6.78680000659775,3.8716090579534));
#14844=CARTESIAN_POINT('Ctrl Pts',(5.90043765469484,6.76643101559881,4.11867588537419));
#14845=CARTESIAN_POINT('Ctrl Pts',(5.77356623131722,6.7478962216523,4.30433440185149));
#14846=CARTESIAN_POINT('Ctrl Pts',(5.59386479707093,6.73115456608272,4.39041942156343));
#14847=CARTESIAN_POINT('Ctrl Pts',(5.44539655895096,6.71866722776999,4.39036886564142));
#14848=CARTESIAN_POINT('Ctrl Pts',(5.33579942713953,6.70871882259051,4.35189016716179));
#14849=CARTESIAN_POINT('Ctrl Pts',(5.23771902383275,6.69879786668875,4.2903366305777));
#14850=CARTESIAN_POINT('Ctrl Pts',(5.14611136868914,6.686446054238,4.17544171847082));
#14851=CARTESIAN_POINT('Ctrl Pts',(5.10728479879167,6.67170559659797,4.00445121458595));
#14852=CARTESIAN_POINT('Ctrl Pts',(5.14611211950831,6.65704405744421,3.83444276345394));
#14853=CARTESIAN_POINT('Ctrl Pts',(5.25438505285132,6.64245966977581,3.69887894687364));
#14854=CARTESIAN_POINT('Ctrl Pts',(5.40990166233343,6.62795227611534,3.62410389391192));
#14855=CARTESIAN_POINT('Ctrl Pts',(5.5815496819327,6.61351997914256,3.62420401324371));
#14856=CARTESIAN_POINT('Ctrl Pts',(5.73544946394382,6.59916119992895,3.69841415911542));
#14857=CARTESIAN_POINT('Ctrl Pts',(5.84118479017196,6.58487472963496,3.83131690200048));
#14858=CARTESIAN_POINT('Ctrl Pts',(5.88325122365517,6.56907782799123,4.01459123943289));
#14859=CARTESIAN_POINT('Ctrl Pts',(5.82128683856772,6.55180183670017,4.21474716794292));
#14860=CARTESIAN_POINT('Ctrl Pts',(5.65822534686918,6.53463077872286,4.34442789266045));
#14861=CARTESIAN_POINT('Ctrl Pts',(5.51207474544734,6.52220844326274,4.36609029268673));
#14862=CARTESIAN_POINT('Ctrl Pts',(5.38742554303644,6.51137100417828,4.34733263783343));
#14863=CARTESIAN_POINT('Ctrl Pts',(5.27165764889733,6.50056364797766,4.2915430638631));
#14864=CARTESIAN_POINT('Ctrl Pts',(5.16905588565897,6.48672787446753,4.16279863377245));
#14865=CARTESIAN_POINT('Ctrl Pts',(5.13283917983621,6.47294482309939,4.00299700475136));
#14866=CARTESIAN_POINT('Ctrl Pts',(5.1750114352257,6.45692788066795,3.81720051065741));
#14867=CARTESIAN_POINT('Ctrl Pts',(5.33289108133986,6.43870149704958,3.65876416560081));
#14868=CARTESIAN_POINT('Ctrl Pts',(5.55419693287486,6.42057082795549,3.63430277213249));
#14869=CARTESIAN_POINT('Ctrl Pts',(5.71118304201485,6.40589452371311,3.71057513225082));
#14870=CARTESIAN_POINT('Ctrl Pts',(5.81726355608341,6.39238507064568,3.82897080987877));
#14871=CARTESIAN_POINT('Ctrl Pts',(5.85858981339439,6.38003097260466,3.97213930596044));
#14872=CARTESIAN_POINT('Ctrl Pts',(5.83401059568513,6.36771004387122,4.11499949089278));
#14873=CARTESIAN_POINT('Ctrl Pts',(5.75793177724685,6.35429201109606,4.25337987346692));
#14874=CARTESIAN_POINT('Ctrl Pts',(5.5841434597572,6.33755678598937,4.36270673919398));
#14875=CARTESIAN_POINT('Ctrl Pts',(5.33972856653595,6.31752970311076,4.33506481527608));
#14876=CARTESIAN_POINT('Ctrl Pts',(5.16631525257735,6.29754423858894,4.16154035829682));
#14877=CARTESIAN_POINT('Ctrl Pts',(5.1389670014894,6.27759361927993,3.91823011012584));
#14878=CARTESIAN_POINT('Ctrl Pts',(5.26923427006138,6.25765586167643,3.71098251993868));
#14879=CARTESIAN_POINT('Ctrl Pts',(5.49997414943137,6.2377376533677,3.63028623162157));
#14880=CARTESIAN_POINT('Ctrl Pts',(5.69234045845551,6.2211328327069,3.69754386482986));
#14881=CARTESIAN_POINT('Ctrl Pts',(5.77889109313146,6.21006107345164,3.79495147685565));
#14882=CARTESIAN_POINT('Ctrl Pts',(5.8287628675858,6.20120152181681,3.88499526513206));
#14883=CARTESIAN_POINT('Ctrl Pts',(5.85505659115829,6.1912298978419,4.00053965484459));
#14884=CARTESIAN_POINT('Ctrl Pts',(5.81423820297505,6.17570552245903,4.18084805030103));
#14885=CARTESIAN_POINT('Ctrl Pts',(5.68925420776868,6.16126646712905,4.3060653674419));
#14886=CARTESIAN_POINT('Ctrl Pts',(5.53801582331833,6.14791748162507,4.34914806893716));
#14887=CARTESIAN_POINT('Ctrl Pts',(5.40729475179393,6.13677964483745,4.34202352685408));
#14888=CARTESIAN_POINT('Ctrl Pts',(5.27577798314163,6.12450821845862,4.27866007683168));
#14889=CARTESIAN_POINT('Ctrl Pts',(5.17621152498865,6.11109298436855,4.15400034396759));
#14890=CARTESIAN_POINT('Ctrl Pts',(5.14062815757453,6.09764920528476,3.99810258706931));
#14891=CARTESIAN_POINT('Ctrl Pts',(5.17621864961869,6.08416957526783,3.84175996625641));
#14892=CARTESIAN_POINT('Ctrl Pts',(5.27645693346059,6.07065378662253,3.71612247842351));
#14893=CARTESIAN_POINT('Ctrl Pts',(5.4216736508846,6.05709829175107,3.64600249711584));
#14894=CARTESIAN_POINT('Ctrl Pts',(5.55642697968229,6.04576775227701,3.64603929507313));
#14895=CARTESIAN_POINT('Ctrl Pts',(5.6440193761318,6.03781700092045,3.67675205629796));
#14896=CARTESIAN_POINT('Ctrl Pts',(5.69026902046296,6.03326803369609,3.70231145507745));
#14897=CARTESIAN_POINT('Ctrl Pts',(5.75500475915597,6.02643854964378,3.74819976516779));
#14898=CARTESIAN_POINT('Ctrl Pts',(5.83113812206107,6.01617049150737,3.84365344915576));
#14899=CARTESIAN_POINT('Ctrl Pts',(5.86766196956311,6.00242939725551,4.00298279625502));
#14900=CARTESIAN_POINT('Ctrl Pts',(5.8311547471775,5.98863491997195,4.16292338324265));
#14901=CARTESIAN_POINT('Ctrl Pts',(5.73709557243115,5.97593951486642,4.28108823702175));
#14902=CARTESIAN_POINT('Ctrl Pts',(5.61781643785115,5.96435631741718,4.34688070547426));
#14903=CARTESIAN_POINT('Ctrl Pts',(5.45603306860374,5.95041149725462,4.37482578814888));
#14904=CARTESIAN_POINT('Ctrl Pts',(5.25316590304169,5.93289348529237,4.30421133407663));
#14905=CARTESIAN_POINT('Ctrl Pts',(5.114334341813,5.91172572229907,4.08431983563909));
#14906=CARTESIAN_POINT('Ctrl Pts',(5.14347742913921,5.89040379142845,3.82415207297242));
#14907=CARTESIAN_POINT('Ctrl Pts',(5.32958757437269,5.8689234097876,3.63744549574417));
#14908=CARTESIAN_POINT('Ctrl Pts',(5.593792158646,5.84727920751737,3.60729146399766));
#14909=CARTESIAN_POINT('Ctrl Pts',(5.78261609629093,5.82909825547531,3.72587469920206));
#14910=CARTESIAN_POINT('Ctrl Pts',(5.86569002809564,5.81446997132799,3.87675017989571));
#14911=CARTESIAN_POINT('Ctrl Pts',(5.88026841209617,5.80712385602455,3.96181257456008));
#14912=CARTESIAN_POINT('Ctrl Pts',(5.88027418431338,5.80344650399414,4.00459648223716));
#14913=CARTESIAN_POINT('Ctrl Pts',(5.95590306687186,7.03727919710367,3.99891416684745));
#14914=CARTESIAN_POINT('Ctrl Pts',(5.95589616141154,7.03287988693566,4.05009764838621));
#14915=CARTESIAN_POINT('Ctrl Pts',(5.93842634741758,7.02407009585036,4.15210152738218));
#14916=CARTESIAN_POINT('Ctrl Pts',(5.83862476994702,7.00647265914313,4.33368324484612));
#14917=CARTESIAN_POINT('Ctrl Pts',(5.61038748339536,6.98450279632803,4.47695533665323));
#14918=CARTESIAN_POINT('Ctrl Pts',(5.28951816532253,6.95820805223714,4.44078048995406));
#14919=CARTESIAN_POINT('Ctrl Pts',(5.06216227665699,6.931985960868,4.21299691146494));
#14920=CARTESIAN_POINT('Ctrl Pts',(5.02611958609637,6.90584826166672,3.89414010003615));
#14921=CARTESIAN_POINT('Ctrl Pts',(5.19653980841186,6.87980141769972,3.62350837417727));
#14922=CARTESIAN_POINT('Ctrl Pts',(5.49724448642999,6.85385971296279,3.5184785366482));
#14923=CARTESIAN_POINT('Ctrl Pts',(5.78525918241898,6.82898632949769,3.61969120955249));
#14924=CARTESIAN_POINT('Ctrl Pts',(5.94765088502646,6.80517631696329,3.85861234902237));
#14925=CARTESIAN_POINT('Ctrl Pts',(5.94772393662232,6.7824215728438,4.1346057376524));
#14926=CARTESIAN_POINT('Ctrl Pts',(5.8057000315009,6.76166065837722,4.34261111889119));
#14927=CARTESIAN_POINT('Ctrl Pts',(5.60401485141267,6.74286906514136,4.4392793038978));
#14928=CARTESIAN_POINT('Ctrl Pts',(5.43709628111368,6.72882975921881,4.43925283529324));
#14929=CARTESIAN_POINT('Ctrl Pts',(5.3137380044414,6.71763253999929,4.39594951157785));
#14930=CARTESIAN_POINT('Ctrl Pts',(5.20326509995367,6.70645831516364,4.32662502497686));
#14931=CARTESIAN_POINT('Ctrl Pts',(5.09996040114962,6.69253290488073,4.19710330322307));
#14932=CARTESIAN_POINT('Ctrl Pts',(5.05610887744417,6.67589443882275,4.0040968779241));
#14933=CARTESIAN_POINT('Ctrl Pts',(5.09995854584184,6.65932883970079,3.8119966041178));
#14934=CARTESIAN_POINT('Ctrl Pts',(5.22238370498492,6.64283754317385,3.65868097433416));
#14935=CARTESIAN_POINT('Ctrl Pts',(5.39835972294708,6.62642245590569,3.57405122274256));
#14936=CARTESIAN_POINT('Ctrl Pts',(5.59268901758044,6.61008477200057,3.57415252520102));
#14937=CARTESIAN_POINT('Ctrl Pts',(5.7669805856365,6.5938259218282,3.6581859819855));
#14938=CARTESIAN_POINT('Ctrl Pts',(5.88673791828364,6.57764687866966,3.80870886087705));
#14939=CARTESIAN_POINT('Ctrl Pts',(5.93438063104257,6.55976041103417,4.01626669154502));
#14940=CARTESIAN_POINT('Ctrl Pts',(5.8642069662864,6.54020125406153,4.24287570953169));
#14941=CARTESIAN_POINT('Ctrl Pts',(5.6797098229945,6.520777947123,4.3895696010608));
#14942=CARTESIAN_POINT('Ctrl Pts',(5.51451149302123,6.50673855146733,4.41403838239402));
#14943=CARTESIAN_POINT('Ctrl Pts',(5.37370646222636,6.49449746275024,4.39284888630218));
#14944=CARTESIAN_POINT('Ctrl Pts',(5.24303700980646,6.48230054675382,4.32985873556225));
#14945=CARTESIAN_POINT('Ctrl Pts',(5.12738220646008,6.46670249550793,4.18469192949528));
#14946=CARTESIAN_POINT('Ctrl Pts',(5.08664089228909,6.4511905915314,4.00479453396285));
#14947=CARTESIAN_POINT('Ctrl Pts',(5.13407589369759,6.43319124323249,3.7959812029093));
#14948=CARTESIAN_POINT('Ctrl Pts',(5.31118286959745,6.41276495133761,3.61841802211263));
#14949=CARTESIAN_POINT('Ctrl Pts',(5.55853958666605,6.39250501417649,3.59122528508859));
#14950=CARTESIAN_POINT('Ctrl Pts',(5.73342093935756,6.37615866441498,3.67625437042241));
#14951=CARTESIAN_POINT('Ctrl Pts',(5.85133313713545,6.36113952640084,3.80790529683591));
#14952=CARTESIAN_POINT('Ctrl Pts',(5.89706702481703,6.34745121016953,3.96663113427204));
#14953=CARTESIAN_POINT('Ctrl Pts',(5.86987038418826,6.33383538334179,4.12451552814598));
#14954=CARTESIAN_POINT('Ctrl Pts',(5.78594882016984,6.31904256295841,4.27708653025637));
#14955=CARTESIAN_POINT('Ctrl Pts',(5.59494613134684,6.30066694840301,4.39701695335078));
#14956=CARTESIAN_POINT('Ctrl Pts',(5.32792628430838,6.2787914117074,4.36655869826738));
#14957=CARTESIAN_POINT('Ctrl Pts',(5.13973148170606,6.25708954605818,4.17786422412083));
#14958=CARTESIAN_POINT('Ctrl Pts',(5.11048151266317,6.23555198387054,3.91512091298944));
#14959=CARTESIAN_POINT('Ctrl Pts',(5.25045794049214,6.21418524204142,3.69297296555494));
#14960=CARTESIAN_POINT('Ctrl Pts',(5.49641917714145,6.19296358963855,3.60727428386931));
#14961=CARTESIAN_POINT('Ctrl Pts',(5.69983988901561,6.17540944769186,3.67867241225569));
#14962=CARTESIAN_POINT('Ctrl Pts',(5.79086497922878,6.16376212897976,3.78118818554554));
#14963=CARTESIAN_POINT('Ctrl Pts',(5.84321117645942,6.15446420449365,3.87570466796909));
#14964=CARTESIAN_POINT('Ctrl Pts',(5.87065814437396,6.14403327021692,3.99661498745638));
#14965=CARTESIAN_POINT('Ctrl Pts',(5.82805008788353,6.12787459541677,4.18430575396648));
#14966=CARTESIAN_POINT('Ctrl Pts',(5.69862866856204,6.11295020903452,4.31365122027558));
#14967=CARTESIAN_POINT('Ctrl Pts',(5.54313378493208,6.0992304546001,4.35787902005905));
#14968=CARTESIAN_POINT('Ctrl Pts',(5.40926178871448,6.08782855308313,4.35054539341534));
#14969=CARTESIAN_POINT('Ctrl Pts',(5.27525709486542,6.07532528539318,4.28587506508975));
#14970=CARTESIAN_POINT('Ctrl Pts',(5.17439041177087,6.06173195224338,4.15944267362621));
#14971=CARTESIAN_POINT('Ctrl Pts',(5.13861259214682,6.04817811425488,4.00222176271348));
#14972=CARTESIAN_POINT('Ctrl Pts',(5.17439053825513,6.03466753046012,3.84546673219833));
#14973=CARTESIAN_POINT('Ctrl Pts',(5.27444029713,6.0211930273313,3.72023060681213));
#14974=CARTESIAN_POINT('Ctrl Pts',(5.41852484284517,6.00775286378202,3.65076614242221));
#14975=CARTESIAN_POINT('Ctrl Pts',(5.55146977058118,5.99657679058691,3.65088710095702));
#14976=CARTESIAN_POINT('Ctrl Pts',(5.63753376629596,5.98876512785074,3.68107859235753));
#14977=CARTESIAN_POINT('Ctrl Pts',(5.68288882480457,5.98430436242261,3.70614602139524));
#14978=CARTESIAN_POINT('Ctrl Pts',(5.74628736488937,5.97761664176628,3.75108884668273));
#14979=CARTESIAN_POINT('Ctrl Pts',(5.82053438649198,5.96759894686408,3.84429050484334));
#14980=CARTESIAN_POINT('Ctrl Pts',(5.8559045113389,5.9542634039028,3.9989889909768));
#14981=CARTESIAN_POINT('Ctrl Pts',(5.82055051327847,5.94094654736442,4.15342083439052));
#14982=CARTESIAN_POINT('Ctrl Pts',(5.7301138579932,5.92875253598539,4.2668953204214));
#14983=CARTESIAN_POINT('Ctrl Pts',(5.61600089164756,5.91767493945766,4.32978774586891));
#14984=CARTESIAN_POINT('Ctrl Pts',(5.46180933263781,5.90438928265866,4.35636097149178));
#14985=CARTESIAN_POINT('Ctrl Pts',(5.26964185338532,5.88779310902171,4.28920833470193));
#14986=CARTESIAN_POINT('Ctrl Pts',(5.13926593838416,5.86788359492209,4.0821491463144));
#14987=CARTESIAN_POINT('Ctrl Pts',(5.1667763249041,5.84797174518985,3.83909164331259));
#14988=CARTESIAN_POINT('Ctrl Pts',(5.33971434420192,5.82804129686562,3.66595696613271));
#14989=CARTESIAN_POINT('Ctrl Pts',(5.58345731087934,5.8080821094971,3.63840397287366));
#14990=CARTESIAN_POINT('Ctrl Pts',(5.75648703078364,5.79142038910681,3.74728751079694));
#14991=CARTESIAN_POINT('Ctrl Pts',(5.83232118693006,5.77805963303851,3.88511710631332));
#14992=CARTESIAN_POINT('Ctrl Pts',(5.84558001546802,5.77137200360298,3.96257247922028));
#14993=CARTESIAN_POINT('Ctrl Pts',(5.8455852749944,5.76802127557217,4.00155630169246));
#14994=CARTESIAN_POINT('Ctrl Pts',(5.94467745847827,7.085541872266,4.00306091406361));
#14995=CARTESIAN_POINT('Ctrl Pts',(5.94467071320255,7.08124461202357,4.05305710253085));
#14996=CARTESIAN_POINT('Ctrl Pts',(5.92762764874893,7.07263818921979,4.15272355020168));
#14997=CARTESIAN_POINT('Ctrl Pts',(5.82985601806925,7.05538712363623,4.33077138583792));
#14998=CARTESIAN_POINT('Ctrl Pts',(5.60523592604193,7.03375625002402,4.47208979961085));
#14999=CARTESIAN_POINT('Ctrl Pts',(5.28717136811017,7.0076963147076,4.43657742893708));
#15000=CARTESIAN_POINT('Ctrl Pts',(5.06016846049025,6.98154572659498,4.20960102607602));
#15001=CARTESIAN_POINT('Ctrl Pts',(5.02365602163957,6.95531367050233,3.8895921954164));
#15002=CARTESIAN_POINT('Ctrl Pts',(5.19551794912881,6.92901180249481,3.61604266611656));
#15003=CARTESIAN_POINT('Ctrl Pts',(5.50106527788403,6.90264790572184,3.50895870577898));
#15004=CARTESIAN_POINT('Ctrl Pts',(5.79577161674239,6.87721212889977,3.61217861137834));
#15005=CARTESIAN_POINT('Ctrl Pts',(5.96305449537282,6.85271938331077,3.85785645038935));
#15006=CARTESIAN_POINT('Ctrl Pts',(5.96336129173779,6.82918177238479,4.14336056358693));
#15007=CARTESIAN_POINT('Ctrl Pts',(5.81582158193089,6.8075910527215,4.35981776235806));
#15008=CARTESIAN_POINT('Ctrl Pts',(5.60511420817303,6.78795692457779,4.46092931066051));
#15009=CARTESIAN_POINT('Ctrl Pts',(5.43000786563227,6.7732300740845,4.4609734353019));
#15010=CARTESIAN_POINT('Ctrl Pts',(5.30020839954856,6.76144926677095,4.41542525093647));
#15011=CARTESIAN_POINT('Ctrl Pts',(5.18374235150296,6.74966952273624,4.34235663912504));
#15012=CARTESIAN_POINT('Ctrl Pts',(5.07447092113825,6.73494816191923,4.20547111387009));
#15013=CARTESIAN_POINT('Ctrl Pts',(5.02784718599889,6.71729065774043,4.00065747110974));
#15014=CARTESIAN_POINT('Ctrl Pts',(5.07447386054353,6.69964459568449,3.79601025923107));
#15015=CARTESIAN_POINT('Ctrl Pts',(5.20529905681373,6.68201315439094,3.63204273671346));
#15016=CARTESIAN_POINT('Ctrl Pts',(5.39408590362551,6.66439961395901,3.54116301717729));
#15017=CARTESIAN_POINT('Ctrl Pts',(5.60333609396693,6.64680714416216,3.54119434056683));
#15018=CARTESIAN_POINT('Ctrl Pts',(5.7916924204204,6.62923879520195,3.63192246515604));
#15019=CARTESIAN_POINT('Ctrl Pts',(5.92158289603545,6.61169790649974,3.79506746854736));
#15020=CARTESIAN_POINT('Ctrl Pts',(5.97348422705736,6.59224132115423,4.0208010865485));
#15021=CARTESIAN_POINT('Ctrl Pts',(5.89702584711254,6.57088802899332,4.2682427919361));
#15022=CARTESIAN_POINT('Ctrl Pts',(5.69487546676521,6.54959462586925,4.42916632782277));
#15023=CARTESIAN_POINT('Ctrl Pts',(5.51317481886798,6.53415151193397,4.45613715780873));
#15024=CARTESIAN_POINT('Ctrl Pts',(5.35801698637868,6.52066195925173,4.43279204584114));
#15025=CARTESIAN_POINT('Ctrl Pts',(5.21374009576453,6.50719519620621,4.36329408523511));
#15026=CARTESIAN_POINT('Ctrl Pts',(5.08567798395226,6.48992954163975,4.20264939874256));
#15027=CARTESIAN_POINT('Ctrl Pts',(5.04041661933432,6.47271281314042,4.00302390822556));
#15028=CARTESIAN_POINT('Ctrl Pts',(5.09312070125709,6.45268959111598,3.770743151734));
#15029=CARTESIAN_POINT('Ctrl Pts',(5.29058645351125,6.42989526702207,3.57256208940533));
#15030=CARTESIAN_POINT('Ctrl Pts',(5.56736489827577,6.40722162609742,3.54199581368896));
#15031=CARTESIAN_POINT('Ctrl Pts',(5.76353539464181,6.38888263494561,3.63733190145256));
#15032=CARTESIAN_POINT('Ctrl Pts',(5.89598723312259,6.37201371483763,3.78518032709043));
#15033=CARTESIAN_POINT('Ctrl Pts',(5.94748358103074,6.35660808187041,3.96374439081115));
#15034=CARTESIAN_POINT('Ctrl Pts',(5.91685865376627,6.34126760667545,4.14161364905986));
#15035=CARTESIAN_POINT('Ctrl Pts',(5.82224248057764,6.32458502365897,4.31366053046754));
#15036=CARTESIAN_POINT('Ctrl Pts',(5.60660953292401,6.30382997132046,4.44913008611416));
#15037=CARTESIAN_POINT('Ctrl Pts',(5.30470259158896,6.27909158348978,4.41475311910331));
#15038=CARTESIAN_POINT('Ctrl Pts',(5.09170051369519,6.25452341621551,4.20123511708807));
#15039=CARTESIAN_POINT('Ctrl Pts',(5.05856247602295,6.23013365457353,3.90374222299026));
#15040=CARTESIAN_POINT('Ctrl Pts',(5.21710547478983,6.20591600947063,3.65215819590566));
#15041=CARTESIAN_POINT('Ctrl Pts',(5.4955522329887,6.18189025349015,3.55516775542111));
#15042=CARTESIAN_POINT('Ctrl Pts',(5.72567785231775,6.16201826770261,3.63598206917989));
#15043=CARTESIAN_POINT('Ctrl Pts',(5.82854913820436,6.14885155715524,3.75185257807874));
#15044=CARTESIAN_POINT('Ctrl Pts',(5.88768132090037,6.13834655444601,3.85862649586901));
#15045=CARTESIAN_POINT('Ctrl Pts',(5.91865398757851,6.12656716972265,3.99513809825376));
#15046=CARTESIAN_POINT('Ctrl Pts',(5.87056737474013,6.10834280183518,4.20678461191633));
#15047=CARTESIAN_POINT('Ctrl Pts',(5.72480600833643,6.09153123535025,4.35234929299144));
#15048=CARTESIAN_POINT('Ctrl Pts',(5.55008041460532,6.07610979937891,4.40202024202591));
#15049=CARTESIAN_POINT('Ctrl Pts',(5.39986618875751,6.06331159280831,4.3937717269471));
#15050=CARTESIAN_POINT('Ctrl Pts',(5.24977367075476,6.04930117532489,4.32130130885873));
#15051=CARTESIAN_POINT('Ctrl Pts',(5.1370759222932,6.03410042382611,4.17994965722586));
#15052=CARTESIAN_POINT('Ctrl Pts',(5.09722624552166,6.0189859086027,4.00464345758488));
#15053=CARTESIAN_POINT('Ctrl Pts',(5.13708274489156,6.00395199588207,3.83031021460055));
#15054=CARTESIAN_POINT('Ctrl Pts',(5.24808791700962,5.98900127852958,3.6914414666054));
#15055=CARTESIAN_POINT('Ctrl Pts',(5.40745664968594,5.97413206983575,3.61467943867966));
#15056=CARTESIAN_POINT('Ctrl Pts',(5.55399870251856,5.96180976298947,3.61486056493999));
#15057=CARTESIAN_POINT('Ctrl Pts',(5.64862248135238,5.95321954864974,3.6480666103073));
#15058=CARTESIAN_POINT('Ctrl Pts',(5.69842524536096,5.94832094967742,3.67559303366571));
#15059=CARTESIAN_POINT('Ctrl Pts',(5.76798070022639,5.94098275227965,3.72490537830438));
#15060=CARTESIAN_POINT('Ctrl Pts',(5.84923025676308,5.93001063189764,3.82698024714553));
#15061=CARTESIAN_POINT('Ctrl Pts',(5.88773532824436,5.91545880053051,3.99575027454172));
#15062=CARTESIAN_POINT('Ctrl Pts',(5.84925547744142,5.9009828238771,4.1635444551542));
#15063=CARTESIAN_POINT('Ctrl Pts',(5.7513255464219,5.88778222195693,4.28630739949125));
#15064=CARTESIAN_POINT('Ctrl Pts',(5.6282755026934,5.87583551525214,4.35409079257078));
#15065=CARTESIAN_POINT('Ctrl Pts',(5.46253669380234,5.86155308506761,4.38260610594922));
#15066=CARTESIAN_POINT('Ctrl Pts',(5.25709446927773,5.84379840048457,4.31056950119396));
#15067=CARTESIAN_POINT('Ctrl Pts',(5.1188863731938,5.8226444314236,4.09047085545772));
#15068=CARTESIAN_POINT('Ctrl Pts',(5.14821797566417,5.80163306758262,3.83419489648604));
#15069=CARTESIAN_POINT('Ctrl Pts',(5.32948302926564,5.78076121516305,3.65319222396216));
#15070=CARTESIAN_POINT('Ctrl Pts',(5.58272277651973,5.76001882939718,3.62490963002238));
#15071=CARTESIAN_POINT('Ctrl Pts',(5.76094172440336,5.74283538634389,3.73734906526789));
#15072=CARTESIAN_POINT('Ctrl Pts',(5.83858054429191,5.72914477225272,3.8785842544305));
#15073=CARTESIAN_POINT('Ctrl Pts',(5.8520911023979,5.72232128177237,3.95760364160119));
#15074=CARTESIAN_POINT('Ctrl Pts',(5.85209646263188,5.71890639514741,3.99733391297083));
#15075=CARTESIAN_POINT('Ctrl Pts',(5.9149593871984,7.09981632447119,4.00428381887363));
#15076=CARTESIAN_POINT('Ctrl Pts',(5.91495308543952,7.0958016186183,4.05099264708924));
#15077=CARTESIAN_POINT('Ctrl Pts',(5.89904039139162,7.08776451910168,4.14406609975579));
#15078=CARTESIAN_POINT('Ctrl Pts',(5.80762376136514,7.07163070606742,4.31058337466593));
#15079=CARTESIAN_POINT('Ctrl Pts',(5.59721423545493,7.05136306306487,4.44307682955313));
#15080=CARTESIAN_POINT('Ctrl Pts',(5.29839493635342,7.02688072250891,4.40985935994832));
#15081=CARTESIAN_POINT('Ctrl Pts',(5.08441495345513,7.00224296763148,4.19612662281291));
#15082=CARTESIAN_POINT('Ctrl Pts',(5.04974875241047,6.97745444355743,3.89375224127796));
#15083=CARTESIAN_POINT('Ctrl Pts',(5.21250981495705,6.95252140927353,3.63434621044489));
#15084=CARTESIAN_POINT('Ctrl Pts',(5.50304341273993,6.9274480281682,3.5323300193668));
#15085=CARTESIAN_POINT('Ctrl Pts',(5.78434555072646,6.90317511570346,3.6306649383391));
#15086=CARTESIAN_POINT('Ctrl Pts',(5.94463823132403,6.87972443166664,3.86582463725867));
#15087=CARTESIAN_POINT('Ctrl Pts',(5.94506874025421,6.85711505479382,4.14007773066394));
#15088=CARTESIAN_POINT('Ctrl Pts',(5.80298180027145,6.83630820453566,4.34876669420255));
#15089=CARTESIAN_POINT('Ctrl Pts',(5.5993330098206,6.81733128287079,4.44656967130991));
#15090=CARTESIAN_POINT('Ctrl Pts',(5.42963725623126,6.80306132062808,4.44666183830942));
#15091=CARTESIAN_POINT('Ctrl Pts',(5.30359323362781,6.79162260587336,4.40244344229727));
#15092=CARTESIAN_POINT('Ctrl Pts',(5.19034833118513,6.78016936879213,4.33140732330614));
#15093=CARTESIAN_POINT('Ctrl Pts',(5.08385604486381,6.76583190694975,4.19809246217554));
#15094=CARTESIAN_POINT('Ctrl Pts',(5.03825146773315,6.74858505106259,3.99803805883399));
#15095=CARTESIAN_POINT('Ctrl Pts',(5.08385657844574,6.73130389443769,3.79758257367279));
#15096=CARTESIAN_POINT('Ctrl Pts',(5.21228621879808,6.71399268838207,3.63650910211638));
#15097=CARTESIAN_POINT('Ctrl Pts',(5.39817377695134,6.69665086519213,3.54694964375529));
#15098=CARTESIAN_POINT('Ctrl Pts',(5.60480938276286,6.67928251587732,3.54691321479687));
#15099=CARTESIAN_POINT('Ctrl Pts',(5.79136032917417,6.66189043106636,3.63669165399195));
#15100=CARTESIAN_POINT('Ctrl Pts',(5.92039378666778,6.64447639659799,3.798656873621));
#15101=CARTESIAN_POINT('Ctrl Pts',(5.97215579848303,6.62510974481235,4.02340656085786));
#15102=CARTESIAN_POINT('Ctrl Pts',(5.89590223862252,6.60377676600798,4.27066947166225));
#15103=CARTESIAN_POINT('Ctrl Pts',(5.69328362721486,6.58243024014988,4.43216184340459));
#15104=CARTESIAN_POINT('Ctrl Pts',(5.51047755263859,6.56689647414804,4.45935690682349));
#15105=CARTESIAN_POINT('Ctrl Pts',(5.35407501259111,6.5533004896361,4.43583123820807));
#15106=CARTESIAN_POINT('Ctrl Pts',(5.20835461031678,6.53970490291349,4.36569371401464));
#15107=CARTESIAN_POINT('Ctrl Pts',(5.07860298299557,6.52221993385381,4.20304133979497));
#15108=CARTESIAN_POINT('Ctrl Pts',(5.03257499448107,6.50474274920277,4.00032758858315));
#15109=CARTESIAN_POINT('Ctrl Pts',(5.08616781619013,6.48435453861134,3.76376359272689));
#15110=CARTESIAN_POINT('Ctrl Pts',(5.28778842673841,6.46107782796493,3.56112334924671));
#15111=CARTESIAN_POINT('Ctrl Pts',(5.57177694710294,6.43781826428389,3.52956237290512));
#15112=CARTESIAN_POINT('Ctrl Pts',(5.77378591102479,6.4189467241674,3.62766025014304));
#15113=CARTESIAN_POINT('Ctrl Pts',(5.91050945448788,6.40153607632419,3.78023093558462));
#15114=CARTESIAN_POINT('Ctrl Pts',(5.96387927126282,6.38560528324312,3.96495886197815));
#15115=CARTESIAN_POINT('Ctrl Pts',(5.93213495257581,6.36969190270551,4.14951323780822));
#15116=CARTESIAN_POINT('Ctrl Pts',(5.83381323704975,6.35235284740185,4.32837272892742));
#15117=CARTESIAN_POINT('Ctrl Pts',(5.60911648444059,6.33072654274578,4.46973537115468));
#15118=CARTESIAN_POINT('Ctrl Pts',(5.2931718071227,6.30484798080865,4.43396198639303));
#15119=CARTESIAN_POINT('Ctrl Pts',(5.06932425874092,6.27905716144787,4.20984555330695));
#15120=CARTESIAN_POINT('Ctrl Pts',(5.03421828644466,6.25335480389872,3.89629859927553));
#15121=CARTESIAN_POINT('Ctrl Pts',(5.20171418169518,6.22777084145329,3.63015017227696));
#15122=CARTESIAN_POINT('Ctrl Pts',(5.49713289769245,6.2022789177778,3.52707275798132));
#15123=CARTESIAN_POINT('Ctrl Pts',(5.74210439555382,6.18114457050484,3.61295915765088));
#15124=CARTESIAN_POINT('Ctrl Pts',(5.8518682951323,6.16710129700844,3.7365649924753));
#15125=CARTESIAN_POINT('Ctrl Pts',(5.91501706249361,6.15588489652694,3.85058437438587));
#15126=CARTESIAN_POINT('Ctrl Pts',(5.94815875179138,6.1432946488714,3.99652625741968));
#15127=CARTESIAN_POINT('Ctrl Pts',(5.89670996174374,6.12377785850373,4.22323046031872));
#15128=CARTESIAN_POINT('Ctrl Pts',(5.74032627079256,6.10574426054262,4.37953203223293));
#15129=CARTESIAN_POINT('Ctrl Pts',(5.55243898812676,6.08916696227491,4.4329671523606));
#15130=CARTESIAN_POINT('Ctrl Pts',(5.39071604519891,6.07539302167999,4.42410346032364));
#15131=CARTESIAN_POINT('Ctrl Pts',(5.22890883093779,6.0602953077351,4.34599909074473));
#15132=CARTESIAN_POINT('Ctrl Pts',(5.10722454589011,6.04389396153373,4.19343552007192));
#15133=CARTESIAN_POINT('Ctrl Pts',(5.06413039868302,6.02755830971277,4.00393860928497));
#15134=CARTESIAN_POINT('Ctrl Pts',(5.10722831777621,6.01129684192045,3.81527822605878));
#15135=CARTESIAN_POINT('Ctrl Pts',(5.22747548470254,5.995106342901,3.66482621676792));
#15136=CARTESIAN_POINT('Ctrl Pts',(5.40028163714302,5.97898878411569,3.58156898328027));
#15137=CARTESIAN_POINT('Ctrl Pts',(5.55933969240477,5.96561723512518,3.58175740628002));
#15138=CARTESIAN_POINT('Ctrl Pts',(5.66210550300135,5.9562890894632,3.61781790440772));
#15139=CARTESIAN_POINT('Ctrl Pts',(5.71620838528512,5.95096787527999,3.64772140297022));
#15140=CARTESIAN_POINT('Ctrl Pts',(5.79178201838636,5.94299563414587,3.70129807305379));
#15141=CARTESIAN_POINT('Ctrl Pts',(5.88009213765861,5.93107477634743,3.81223105667651));
#15142=CARTESIAN_POINT('Ctrl Pts',(5.92197627191235,5.91525578799805,3.99574650770481));
#15143=CARTESIAN_POINT('Ctrl Pts',(5.88011310439625,5.89951367020608,4.17827551464281));
#15144=CARTESIAN_POINT('Ctrl Pts',(5.77355284379942,5.88515292216243,4.31185923524939));
#15145=CARTESIAN_POINT('Ctrl Pts',(5.63963221810424,5.87215333951234,4.38562554412733));
#15146=CARTESIAN_POINT('Ctrl Pts',(5.45924850580616,5.85661192507217,4.41665712792164));
#15147=CARTESIAN_POINT('Ctrl Pts',(5.23567580323262,5.83729458949201,4.33824620829054));
#15148=CARTESIAN_POINT('Ctrl Pts',(5.08534542689851,5.81428812401155,4.09879386786708));
#15149=CARTESIAN_POINT('Ctrl Pts',(5.11727898328737,5.79145701238181,3.8202071105913));
#15150=CARTESIAN_POINT('Ctrl Pts',(5.31417199281544,5.76879711912542,3.62367687736167));
#15151=CARTESIAN_POINT('Ctrl Pts',(5.58884524217245,5.74630623137894,3.59308087302305));
#15152=CARTESIAN_POINT('Ctrl Pts',(5.78177453472185,5.72770685157949,3.71490177588423));
#15153=CARTESIAN_POINT('Ctrl Pts',(5.86570779175526,5.71290424187196,3.86762747609063));
#15154=CARTESIAN_POINT('Ctrl Pts',(5.88029185858757,5.70553413368606,3.95299047765566));
#15155=CARTESIAN_POINT('Ctrl Pts',(5.88029764289545,5.7018490789545,3.99586400189707));
#15156=CARTESIAN_POINT('Ctrl Pts',(5.89999942231746,7.09981632447119,4.00428180053801));
#15157=CARTESIAN_POINT('Ctrl Pts',(5.89999334367971,7.09594376396835,4.04933684813297));
#15158=CARTESIAN_POINT('Ctrl Pts',(5.88465017335476,7.08819405075721,4.13908165517953));
#15159=CARTESIAN_POINT('Ctrl Pts',(5.7964860030169,7.07263331806119,4.29968204261715));
#15160=CARTESIAN_POINT('Ctrl Pts',(5.59351456200701,7.05308119240215,4.4275031391656));
#15161=CARTESIAN_POINT('Ctrl Pts',(5.30510775645105,7.02945158726801,4.39546636939848));
#15162=CARTESIAN_POINT('Ctrl Pts',(5.09844717527872,7.00565845259414,4.18908156433879));
#15163=CARTESIAN_POINT('Ctrl Pts',(5.06491507736497,6.98170283632427,3.89688445847127));
#15164=CARTESIAN_POINT('Ctrl Pts',(5.22229231109316,6.957587725778,3.64598811283775));
#15165=CARTESIAN_POINT('Ctrl Pts',(5.50350105188817,6.93331581944121,3.54720017800962));
#15166=CARTESIAN_POINT('Ctrl Pts',(5.77606730494162,6.90979543600253,3.64243302852389));
#15167=CARTESIAN_POINT('Ctrl Pts',(5.93155863446605,6.88704927881041,3.87048202703801));
#15168=CARTESIAN_POINT('Ctrl Pts',(5.93201459027321,6.86509833940111,4.13672884061229));
#15169=CARTESIAN_POINT('Ctrl Pts',(5.79395734371705,6.84487476341531,4.33956419787309));
#15170=CARTESIAN_POINT('Ctrl Pts',(5.59585169142646,6.82641140225049,4.43472796239094));
#15171=CARTESIAN_POINT('Ctrl Pts',(5.43062330290708,6.81251496798271,4.43483227755276));
#15172=CARTESIAN_POINT('Ctrl Pts',(5.30781628774365,6.8013693608627,4.39175312056372));
#15173=CARTESIAN_POINT('Ctrl Pts',(5.19743069189207,6.79020509173472,4.32251414855249));
#15174=CARTESIAN_POINT('Ctrl Pts',(5.09353798605695,6.77621535562195,4.1924772803632));
#15175=CARTESIAN_POINT('Ctrl Pts',(5.04898925851302,6.75937456735607,3.99715324700454));
#15176=CARTESIAN_POINT('Ctrl Pts',(5.0935413464267,6.74248271039737,3.80123524176677));
#15177=CARTESIAN_POINT('Ctrl Pts',(5.21917592334569,6.72554188446977,3.64363320271165));
#15178=CARTESIAN_POINT('Ctrl Pts',(5.40122000385758,6.70855426693318,3.55590244763416));
#15179=CARTESIAN_POINT('Ctrl Pts',(5.60380955719718,6.6915221019177,3.55584448787041));
#15180=CARTESIAN_POINT('Ctrl Pts',(5.78691645390742,6.67444770371231,3.64394104146688));
#15181=CARTESIAN_POINT('Ctrl Pts',(5.91372041331327,6.65733344366189,3.80307026683985));
#15182=CARTESIAN_POINT('Ctrl Pts',(5.96466327221314,6.63827601600008,4.02414934139344));
#15183=CARTESIAN_POINT('Ctrl Pts',(5.88961383686182,6.61726302422527,4.26770951451258));
#15184=CARTESIAN_POINT('Ctrl Pts',(5.68975602864846,6.59619863118807,4.42707389952551));
#15185=CARTESIAN_POINT('Ctrl Pts',(5.50916223586277,6.58084997697241,4.45396467698472));
#15186=CARTESIAN_POINT('Ctrl Pts',(5.35453310810722,6.56740673736238,4.43070717074375));
#15187=CARTESIAN_POINT('Ctrl Pts',(5.21033393748589,6.55395079494006,4.36132595428699));
#15188=CARTESIAN_POINT('Ctrl Pts',(5.08177516019845,6.53662851034176,4.20021226638331));
#15189=CARTESIAN_POINT('Ctrl Pts',(5.03609211123456,6.51928717867399,3.99913913108666));
#15190=CARTESIAN_POINT('Ctrl Pts',(5.08928582945947,6.49903664031616,3.76419897777231));
#15191=CARTESIAN_POINT('Ctrl Pts',(5.28978283301087,6.47587070029814,3.56256415950519));
#15192=CARTESIAN_POINT('Ctrl Pts',(5.57279015344961,6.4526862562021,3.53101713469425));
#15193=CARTESIAN_POINT('Ctrl Pts',(5.7744501239661,6.4338421384389,3.62890875798563));
#15194=CARTESIAN_POINT('Ctrl Pts',(5.91107614262552,6.41644569471267,3.78134048060785));
#15195=CARTESIAN_POINT('Ctrl Pts',(5.96451577569518,6.40049895608791,3.96616344909838));
#15196=CARTESIAN_POINT('Ctrl Pts',(5.9327299609379,6.3845554854669,4.15104965949736));
#15197=CARTESIAN_POINT('Ctrl Pts',(5.83415684595966,6.36716688464879,4.33040203531341));
#15198=CARTESIAN_POINT('Ctrl Pts',(5.60855787080152,6.3454421500065,4.47243154476512));
#15199=CARTESIAN_POINT('Ctrl Pts',(5.29067075546292,6.31939963984916,4.43654609473001));
#15200=CARTESIAN_POINT('Ctrl Pts',(5.06495666340114,6.29339375333233,4.21070709279472));
#15201=CARTESIAN_POINT('Ctrl Pts',(5.02940089438198,6.26743382198568,3.89407398616837));
#15202=CARTESIAN_POINT('Ctrl Pts',(5.19880065125732,6.24152902171826,3.62471661866899));
#15203=CARTESIAN_POINT('Ctrl Pts',(5.49820781434257,6.21568834443117,3.52014376389726));
#15204=CARTESIAN_POINT('Ctrl Pts',(5.74701061020189,6.19421520170402,3.60728770872527));
#15205=CARTESIAN_POINT('Ctrl Pts',(5.85863359577984,6.17993370216935,3.73296424281348));
#15206=CARTESIAN_POINT('Ctrl Pts',(5.92288006435656,6.16852118154694,3.84896516413552));
#15207=CARTESIAN_POINT('Ctrl Pts',(5.95664235896203,6.15570021350747,3.99755228818456));
#15208=CARTESIAN_POINT('Ctrl Pts',(5.90422907170185,6.13580438066566,4.22863954557107));
#15209=CARTESIAN_POINT('Ctrl Pts',(5.74463079333177,6.1173884553624,4.38823789360272));
#15210=CARTESIAN_POINT('Ctrl Pts',(5.55259803695828,6.10044178794059,4.44287010078724));
#15211=CARTESIAN_POINT('Ctrl Pts',(5.38717753744307,6.08634982964905,4.43381260797737));
#15212=CARTESIAN_POINT('Ctrl Pts',(5.22149962135128,6.07088880373497,4.35387124517548));
#15213=CARTESIAN_POINT('Ctrl Pts',(5.09676922730111,6.0540743240685,4.197519449458));
#15214=CARTESIAN_POINT('Ctrl Pts',(5.0525318165955,6.03731392845979,4.00312051246728));
#15215=CARTESIAN_POINT('Ctrl Pts',(5.09677460214568,6.02060952469266,3.80936725739853));
#15216=CARTESIAN_POINT('Ctrl Pts',(5.22036100773764,6.00396293698029,3.65469518694587));
#15217=CARTESIAN_POINT('Ctrl Pts',(5.39815221757406,5.98737590584214,3.56901265908242));
#15218=CARTESIAN_POINT('Ctrl Pts',(5.56194673621828,5.9736043825902,3.56918712785721));
#15219=CARTESIAN_POINT('Ctrl Pts',(5.6678409475086,5.96399177625527,3.60634259138081));
#15220=CARTESIAN_POINT('Ctrl Pts',(5.72360710674561,5.9585067948969,3.63716464071472));
#15221=CARTESIAN_POINT('Ctrl Pts',(5.80152037634414,5.9502873075744,3.69239994875946));
#15222=CARTESIAN_POINT('Ctrl Pts',(5.89262775771971,5.93798818799799,3.80682412790902));
#15223=CARTESIAN_POINT('Ctrl Pts',(5.93588165070209,5.9216549676263,3.9962737943898));
#15224=CARTESIAN_POINT('Ctrl Pts',(5.89265315890838,5.90538862230925,4.18485446150754));
#15225=CARTESIAN_POINT('Ctrl Pts',(5.78249899819111,5.89054018760752,4.32296861862104));
#15226=CARTESIAN_POINT('Ctrl Pts',(5.64397324912796,5.87709200642215,4.39928196165792));
#15227=CARTESIAN_POINT('Ctrl Pts',(5.45729571883929,5.86100659113963,4.43140768516966));
#15228=CARTESIAN_POINT('Ctrl Pts',(5.22574876053333,5.84099901355926,4.35024097908663));
#15229=CARTESIAN_POINT('Ctrl Pts',(5.0699063365284,5.81715142001874,4.10208650989737));
#15230=CARTESIAN_POINT('Ctrl Pts',(5.10298913581097,5.79346725679344,3.81314318112568));
#15231=CARTESIAN_POINT('Ctrl Pts',(5.30729513304354,5.76994860790156,3.60917536341897));
#15232=CARTESIAN_POINT('Ctrl Pts',(5.59246492988907,5.74659517888843,3.57738640664907));
#15233=CARTESIAN_POINT('Ctrl Pts',(5.79284572265032,5.72727468967069,3.7038989587173));
#15234=CARTESIAN_POINT('Ctrl Pts',(5.8800308145667,5.71189869700794,3.86253471396896));
#15235=CARTESIAN_POINT('Ctrl Pts',(5.8951821641861,5.70424160396714,3.95121652410008));
#15236=CARTESIAN_POINT('Ctrl Pts',(5.89518817092524,5.70041484319491,3.99573871784903));
#15237=CARTESIAN_POINT('',(5.89999942231746,7.09981632447119,4.00428180053802));
#15238=CARTESIAN_POINT('Origin',(5.9,7.05,4.));
#15239=CARTESIAN_POINT('',(5.89518817092524,5.70041484319491,3.99573871784901));
#15240=CARTESIAN_POINT('Ctrl Pts',(5.89999942231746,7.09981632447119,4.00428180053801));
#15241=CARTESIAN_POINT('Ctrl Pts',(5.89999334367971,7.09594376396835,4.04933684813297));
#15242=CARTESIAN_POINT('Ctrl Pts',(5.88465017335476,7.08819405075721,4.13908165517953));
#15243=CARTESIAN_POINT('Ctrl Pts',(5.7964860030169,7.07263331806119,4.29968204261715));
#15244=CARTESIAN_POINT('Ctrl Pts',(5.59351456200701,7.05308119240215,4.4275031391656));
#15245=CARTESIAN_POINT('Ctrl Pts',(5.30510775645105,7.02945158726801,4.39546636939848));
#15246=CARTESIAN_POINT('Ctrl Pts',(5.09844717527872,7.00565845259414,4.18908156433879));
#15247=CARTESIAN_POINT('Ctrl Pts',(5.06491507736497,6.98170283632427,3.89688445847127));
#15248=CARTESIAN_POINT('Ctrl Pts',(5.22229231109316,6.957587725778,3.64598811283775));
#15249=CARTESIAN_POINT('Ctrl Pts',(5.50350105188817,6.93331581944121,3.54720017800962));
#15250=CARTESIAN_POINT('Ctrl Pts',(5.77606730494162,6.90979543600253,3.64243302852389));
#15251=CARTESIAN_POINT('Ctrl Pts',(5.93155863446605,6.88704927881041,3.87048202703801));
#15252=CARTESIAN_POINT('Ctrl Pts',(5.93201459027321,6.86509833940111,4.13672884061229));
#15253=CARTESIAN_POINT('Ctrl Pts',(5.79395734371705,6.84487476341531,4.33956419787309));
#15254=CARTESIAN_POINT('Ctrl Pts',(5.59585169142646,6.82641140225049,4.43472796239094));
#15255=CARTESIAN_POINT('Ctrl Pts',(5.43062330290708,6.81251496798271,4.43483227755276));
#15256=CARTESIAN_POINT('Ctrl Pts',(5.30781628774365,6.8013693608627,4.39175312056372));
#15257=CARTESIAN_POINT('Ctrl Pts',(5.19743069189207,6.79020509173472,4.32251414855249));
#15258=CARTESIAN_POINT('Ctrl Pts',(5.09353798605695,6.77621535562195,4.1924772803632));
#15259=CARTESIAN_POINT('Ctrl Pts',(5.04898925851302,6.75937456735607,3.99715324700454));
#15260=CARTESIAN_POINT('Ctrl Pts',(5.0935413464267,6.74248271039737,3.80123524176677));
#15261=CARTESIAN_POINT('Ctrl Pts',(5.21917592334569,6.72554188446977,3.64363320271165));
#15262=CARTESIAN_POINT('Ctrl Pts',(5.40122000385758,6.70855426693318,3.55590244763416));
#15263=CARTESIAN_POINT('Ctrl Pts',(5.60380955719718,6.6915221019177,3.55584448787041));
#15264=CARTESIAN_POINT('Ctrl Pts',(5.78691645390742,6.67444770371231,3.64394104146688));
#15265=CARTESIAN_POINT('Ctrl Pts',(5.91372041331327,6.65733344366189,3.80307026683985));
#15266=CARTESIAN_POINT('Ctrl Pts',(5.96466327221314,6.63827601600008,4.02414934139344));
#15267=CARTESIAN_POINT('Ctrl Pts',(5.88961383686182,6.61726302422527,4.26770951451258));
#15268=CARTESIAN_POINT('Ctrl Pts',(5.68975602864846,6.59619863118807,4.42707389952551));
#15269=CARTESIAN_POINT('Ctrl Pts',(5.50916223586277,6.58084997697241,4.45396467698472));
#15270=CARTESIAN_POINT('Ctrl Pts',(5.35453310810722,6.56740673736238,4.43070717074375));
#15271=CARTESIAN_POINT('Ctrl Pts',(5.21033393748589,6.55395079494006,4.36132595428699));
#15272=CARTESIAN_POINT('Ctrl Pts',(5.08177516019845,6.53662851034176,4.20021226638331));
#15273=CARTESIAN_POINT('Ctrl Pts',(5.03609211123456,6.51928717867399,3.99913913108666));
#15274=CARTESIAN_POINT('Ctrl Pts',(5.08928582945947,6.49903664031616,3.76419897777231));
#15275=CARTESIAN_POINT('Ctrl Pts',(5.28978283301087,6.47587070029814,3.56256415950519));
#15276=CARTESIAN_POINT('Ctrl Pts',(5.57279015344961,6.4526862562021,3.53101713469425));
#15277=CARTESIAN_POINT('Ctrl Pts',(5.7744501239661,6.4338421384389,3.62890875798563));
#15278=CARTESIAN_POINT('Ctrl Pts',(5.91107614262552,6.41644569471267,3.78134048060785));
#15279=CARTESIAN_POINT('Ctrl Pts',(5.96451577569518,6.40049895608791,3.96616344909838));
#15280=CARTESIAN_POINT('Ctrl Pts',(5.9327299609379,6.3845554854669,4.15104965949736));
#15281=CARTESIAN_POINT('Ctrl Pts',(5.83415684595966,6.36716688464879,4.33040203531341));
#15282=CARTESIAN_POINT('Ctrl Pts',(5.60855787080152,6.3454421500065,4.47243154476512));
#15283=CARTESIAN_POINT('Ctrl Pts',(5.29067075546292,6.31939963984916,4.43654609473001));
#15284=CARTESIAN_POINT('Ctrl Pts',(5.06495666340114,6.29339375333233,4.21070709279472));
#15285=CARTESIAN_POINT('Ctrl Pts',(5.02940089438198,6.26743382198568,3.89407398616837));
#15286=CARTESIAN_POINT('Ctrl Pts',(5.19880065125732,6.24152902171826,3.62471661866899));
#15287=CARTESIAN_POINT('Ctrl Pts',(5.49820781434257,6.21568834443117,3.52014376389726));
#15288=CARTESIAN_POINT('Ctrl Pts',(5.74701061020189,6.19421520170402,3.60728770872527));
#15289=CARTESIAN_POINT('Ctrl Pts',(5.85863359577984,6.17993370216935,3.73296424281348));
#15290=CARTESIAN_POINT('Ctrl Pts',(5.92288006435656,6.16852118154694,3.84896516413552));
#15291=CARTESIAN_POINT('Ctrl Pts',(5.95664235896203,6.15570021350747,3.99755228818456));
#15292=CARTESIAN_POINT('Ctrl Pts',(5.90422907170185,6.13580438066566,4.22863954557107));
#15293=CARTESIAN_POINT('Ctrl Pts',(5.74463079333177,6.1173884553624,4.38823789360272));
#15294=CARTESIAN_POINT('Ctrl Pts',(5.55259803695828,6.10044178794059,4.44287010078724));
#15295=CARTESIAN_POINT('Ctrl Pts',(5.38717753744307,6.08634982964905,4.43381260797737));
#15296=CARTESIAN_POINT('Ctrl Pts',(5.22149962135128,6.07088880373497,4.35387124517548));
#15297=CARTESIAN_POINT('Ctrl Pts',(5.09676922730111,6.0540743240685,4.197519449458));
#15298=CARTESIAN_POINT('Ctrl Pts',(5.0525318165955,6.03731392845979,4.00312051246728));
#15299=CARTESIAN_POINT('Ctrl Pts',(5.09677460214568,6.02060952469266,3.80936725739853));
#15300=CARTESIAN_POINT('Ctrl Pts',(5.22036100773764,6.00396293698029,3.65469518694587));
#15301=CARTESIAN_POINT('Ctrl Pts',(5.39815221757406,5.98737590584214,3.56901265908242));
#15302=CARTESIAN_POINT('Ctrl Pts',(5.56194673621828,5.9736043825902,3.56918712785721));
#15303=CARTESIAN_POINT('Ctrl Pts',(5.6678409475086,5.96399177625527,3.60634259138081));
#15304=CARTESIAN_POINT('Ctrl Pts',(5.72360710674561,5.9585067948969,3.63716464071472));
#15305=CARTESIAN_POINT('Ctrl Pts',(5.80152037634414,5.9502873075744,3.69239994875946));
#15306=CARTESIAN_POINT('Ctrl Pts',(5.89262775771971,5.93798818799799,3.80682412790902));
#15307=CARTESIAN_POINT('Ctrl Pts',(5.93588165070209,5.9216549676263,3.9962737943898));
#15308=CARTESIAN_POINT('Ctrl Pts',(5.89265315890838,5.90538862230925,4.18485446150754));
#15309=CARTESIAN_POINT('Ctrl Pts',(5.78249899819111,5.89054018760752,4.32296861862104));
#15310=CARTESIAN_POINT('Ctrl Pts',(5.64397324912796,5.87709200642215,4.39928196165792));
#15311=CARTESIAN_POINT('Ctrl Pts',(5.45729571883929,5.86100659113963,4.43140768516966));
#15312=CARTESIAN_POINT('Ctrl Pts',(5.22574876053333,5.84099901355926,4.35024097908663));
#15313=CARTESIAN_POINT('Ctrl Pts',(5.0699063365284,5.81715142001874,4.10208650989737));
#15314=CARTESIAN_POINT('Ctrl Pts',(5.10298913581097,5.79346725679344,3.81314318112568));
#15315=CARTESIAN_POINT('Ctrl Pts',(5.30729513304354,5.76994860790156,3.60917536341897));
#15316=CARTESIAN_POINT('Ctrl Pts',(5.59246492988907,5.74659517888843,3.57738640664907));
#15317=CARTESIAN_POINT('Ctrl Pts',(5.79284572265032,5.72727468967069,3.7038989587173));
#15318=CARTESIAN_POINT('Ctrl Pts',(5.8800308145667,5.71189869700794,3.86253471396896));
#15319=CARTESIAN_POINT('Ctrl Pts',(5.8951821641861,5.70424160396714,3.95121652410008));
#15320=CARTESIAN_POINT('Ctrl Pts',(5.89518817092524,5.70041484319491,3.99573871784903));
#15321=CARTESIAN_POINT('Origin',(5.9,5.75,4.));
#15322=CARTESIAN_POINT('Origin',(5.9,5.75,4.));
#15323=CARTESIAN_POINT('Origin',(5.9,7.05,4.));
#15324=CARTESIAN_POINT('',(0.,0.,0.));
#15325=CARTESIAN_POINT('Origin',(0.375,0.5,0.));
#15326=CARTESIAN_POINT('',(-0.375,0.5,-4.59242549680257E-17));
#15327=CARTESIAN_POINT('Origin',(0.,0.5,0.));
#15328=CARTESIAN_POINT('Origin',(0.,0.475,0.));
#15329=CARTESIAN_POINT('',(-0.425,0.45,-5.20474889637625E-17));
#15330=CARTESIAN_POINT('Origin',(0.,0.45,0.));
#15331=CARTESIAN_POINT('',(-0.4,0.475,-4.89858719658941E-17));
#15332=CARTESIAN_POINT('Origin',(0.,0.24,0.));
#15333=CARTESIAN_POINT('',(-0.425,0.0299999999999998,-5.20474889637625E-17));
#15334=CARTESIAN_POINT('Origin',(0.,0.0299999999999998,0.));
#15335=CARTESIAN_POINT('',(-0.425,0.24,-5.20474889637625E-17));
#15336=CARTESIAN_POINT('Origin',(0.,0.0150000000000001,0.));
#15337=CARTESIAN_POINT('',(-0.395,4.85722573273506E-17,-4.83735485663204E-17));
#15338=CARTESIAN_POINT('Origin',(0.,0.,0.));
#15339=CARTESIAN_POINT('',(-0.41,0.0150000000000001,-5.02105187650415E-17));
#15340=CARTESIAN_POINT('Origin',(0.27,0.,0.));
#15341=CARTESIAN_POINT('',(-0.27,0.,-3.30654635769785E-17));
#15342=CARTESIAN_POINT('Origin',(0.,0.,0.));
#15343=CARTESIAN_POINT('Origin',(0.,-0.02,0.));
#15344=CARTESIAN_POINT('',(-0.24505,-0.0498999999999999,3.00099698131059E-17));
#15345=CARTESIAN_POINT('Origin',(0.,-0.0498999999999999,0.));
#15346=CARTESIAN_POINT('',(-0.26,-0.02,-3.18408167778312E-17));
#15347=CARTESIAN_POINT('Origin',(0.,-0.995,0.));
#15348=CARTESIAN_POINT('',(-0.24505,-1.95495,3.00099698131059E-17));
#15349=CARTESIAN_POINT('Origin',(0.,-1.95495,0.));
#15350=CARTESIAN_POINT('',(-0.24505,-0.995,-3.00099698131059E-17));
#15351=CARTESIAN_POINT('Origin',(0.,-1.975,0.));
#15352=CARTESIAN_POINT('',(-0.2,-2.,-2.44929359829471E-17));
#15353=CARTESIAN_POINT('Origin',(0.,-2.,0.));
#15354=CARTESIAN_POINT('',(-0.225,-1.975,-2.75545529808154E-17));
#15355=CARTESIAN_POINT('Origin',(0.,-2.,0.));
#15356=CARTESIAN_POINT('Origin',(0.115470053837925,-0.5,-0.2));
#15357=CARTESIAN_POINT('',(0.23094010767585,-0.5,0.));
#15358=CARTESIAN_POINT('',(0.115470053837925,-0.5,-0.2));
#15359=CARTESIAN_POINT('',(0.23094010767585,-0.5,0.));
#15360=CARTESIAN_POINT('',(0.115470053837925,-0.8,-0.2));
#15361=CARTESIAN_POINT('',(0.115470053837925,-0.5,-0.2));
#15362=CARTESIAN_POINT('',(0.23094010767585,-0.8,0.));
#15363=CARTESIAN_POINT('',(0.23094010767585,-0.8,0.));
#15364=CARTESIAN_POINT('',(0.23094010767585,-0.5,0.));
#15365=CARTESIAN_POINT('Origin',(-0.115470053837925,-0.5,-0.2));
#15366=CARTESIAN_POINT('',(-0.115470053837925,-0.5,-0.2));
#15367=CARTESIAN_POINT('',(0.115470053837925,-0.5,-0.2));
#15368=CARTESIAN_POINT('',(-0.115470053837925,-0.8,-0.2));
#15369=CARTESIAN_POINT('',(-0.115470053837925,-0.5,-0.2));
#15370=CARTESIAN_POINT('',(0.115470053837925,-0.8,-0.2));
#15371=CARTESIAN_POINT('Origin',(-0.23094010767585,-0.5,-2.77555756156289E-17));
#15372=CARTESIAN_POINT('',(-0.23094010767585,-0.5,-2.82820063659975E-17));
#15373=CARTESIAN_POINT('',(-0.115470053837925,-0.5,-0.2));
#15374=CARTESIAN_POINT('',(-0.23094010767585,-0.8,-2.77555756156289E-17));
#15375=CARTESIAN_POINT('',(-0.23094010767585,-0.5,-2.82820063659975E-17));
#15376=CARTESIAN_POINT('',(-0.115470053837925,-0.8,-0.2));
#15377=CARTESIAN_POINT('Origin',(-0.115470053837925,-0.5,0.2));
#15378=CARTESIAN_POINT('',(-0.115470053837925,-0.5,0.2));
#15379=CARTESIAN_POINT('',(-0.23094010767585,-0.5,-2.82820063659975E-17));
#15380=CARTESIAN_POINT('',(-0.115470053837925,-0.8,0.2));
#15381=CARTESIAN_POINT('',(-0.115470053837925,-0.5,0.2));
#15382=CARTESIAN_POINT('',(-0.23094010767585,-0.8,-2.82820063659975E-17));
#15383=CARTESIAN_POINT('Origin',(0.115470053837925,-0.5,0.2));
#15384=CARTESIAN_POINT('',(0.115470053837925,-0.5,0.2));
#15385=CARTESIAN_POINT('',(-0.115470053837925,-0.5,0.2));
#15386=CARTESIAN_POINT('',(0.115470053837925,-0.8,0.2));
#15387=CARTESIAN_POINT('',(0.115470053837925,-0.5,0.2));
#15388=CARTESIAN_POINT('',(-0.115470053837925,-0.8,0.2));
#15389=CARTESIAN_POINT('Origin',(0.23094010767585,-0.5,0.));
#15390=CARTESIAN_POINT('',(0.115470053837925,-0.5,0.2));
#15391=CARTESIAN_POINT('',(0.115470053837925,-0.8,0.2));
#15392=CARTESIAN_POINT('Origin',(0.,-0.5,0.));
#15393=CARTESIAN_POINT('Origin',(0.,-0.8,0.));
#15394=CARTESIAN_POINT('',(0.,0.,0.));
#15395=CARTESIAN_POINT('',(0.,0.,0.));
#15396=CARTESIAN_POINT('Origin',(0.,0.,0.));
#15397=CARTESIAN_POINT('',(-1.070235,-0.308121667383195,-1.31065986708547E-16));
#15398=CARTESIAN_POINT('',(-1.31065986708547E-16,-0.308121667383195,1.070235));
#15399=CARTESIAN_POINT('Origin',(0.,-0.308121667383195,0.));
#15400=CARTESIAN_POINT('Origin',(0.,-0.308121667383195,0.));
#15401=CARTESIAN_POINT('',(-1.31065986708547E-16,0.308121667383195,1.070235));
#15402=CARTESIAN_POINT('Origin',(-1.34711147906209E-16,0.,1.1));
#15403=CARTESIAN_POINT('',(-1.070235,0.308121667383195,1.31065986708547E-16));
#15404=CARTESIAN_POINT('Origin',(0.,0.308121667383195,0.));
#15405=CARTESIAN_POINT('Origin',(0.,0.308121667383195,0.));
#15406=CARTESIAN_POINT('Origin',(0.,0.,0.));
#15407=CARTESIAN_POINT('',(-1.070235,0.5,-1.31065986708547E-16));
#15408=CARTESIAN_POINT('',(-1.070235,0.,-1.31065986708547E-16));
#15409=CARTESIAN_POINT('Origin',(0.,0.5,0.));
#15410=CARTESIAN_POINT('Origin',(0.,0.,0.));
#15411=CARTESIAN_POINT('',(-0.6,-0.44,-7.34788079488412E-17));
#15412=CARTESIAN_POINT('Origin',(0.,-0.44,0.));
#15413=CARTESIAN_POINT('',(-0.6,0.44,-7.34788079488412E-17));
#15414=CARTESIAN_POINT('',(-0.6,0.,-7.34788079488412E-17));
#15415=CARTESIAN_POINT('Origin',(0.,0.44,0.));
#15416=CARTESIAN_POINT('Origin',(0.,0.47,0.));
#15417=CARTESIAN_POINT('',(-0.66,0.5,-8.08266887437253E-17));
#15418=CARTESIAN_POINT('',(-0.63,0.47,-7.71527483462832E-17));
#15419=CARTESIAN_POINT('Origin',(0.,0.5,0.));
#15420=CARTESIAN_POINT('Origin',(1.070235,0.5,0.));
#15421=CARTESIAN_POINT('Origin',(0.,0.,0.));
#15422=CARTESIAN_POINT('',(-1.070235,-0.5,-1.31065986708547E-16));
#15423=CARTESIAN_POINT('Origin',(0.,-0.5,0.));
#15424=CARTESIAN_POINT('',(-1.070235,0.,-1.31065986708547E-16));
#15425=CARTESIAN_POINT('Origin',(0.66,-0.5,0.));
#15426=CARTESIAN_POINT('',(-0.66,-0.5,-8.08266887437253E-17));
#15427=CARTESIAN_POINT('Origin',(0.,-0.5,0.));
#15428=CARTESIAN_POINT('Origin',(0.,-0.47,0.));
#15429=CARTESIAN_POINT('',(-0.63,-0.47,-7.71527483462832E-17));
#15430=CARTESIAN_POINT('',(0.,0.,0.));
#15431=CARTESIAN_POINT('Origin',(0.,0.,0.));
#15432=CARTESIAN_POINT('',(-1.129765,0.308121667383195,-1.38356309103871E-16));
#15433=CARTESIAN_POINT('',(-1.38356309103871E-16,0.308121667383195,1.129765));
#15434=CARTESIAN_POINT('Origin',(0.,0.308121667383195,0.));
#15435=CARTESIAN_POINT('Origin',(0.,0.308121667383195,0.));
#15436=CARTESIAN_POINT('',(-1.38356309103871E-16,-0.308121667383195,1.129765));
#15437=CARTESIAN_POINT('Origin',(-1.34711147906209E-16,0.,1.1));
#15438=CARTESIAN_POINT('',(-1.129765,-0.308121667383195,1.38356309103871E-16));
#15439=CARTESIAN_POINT('Origin',(0.,-0.308121667383195,0.));
#15440=CARTESIAN_POINT('Origin',(0.,-0.308121667383195,0.));
#15441=CARTESIAN_POINT('Origin',(0.,0.,0.));
#15442=CARTESIAN_POINT('',(-1.129765,-0.5,-1.38356309103871E-16));
#15443=CARTESIAN_POINT('Origin',(0.,-0.5,0.));
#15444=CARTESIAN_POINT('',(-1.129765,0.,-1.38356309103871E-16));
#15445=CARTESIAN_POINT('Origin',(1.54,0.5,0.));
#15446=CARTESIAN_POINT('',(-1.54,0.5,-1.88595607068692E-16));
#15447=CARTESIAN_POINT('Origin',(0.,0.5,0.));
#15448=CARTESIAN_POINT('',(-1.129765,0.5,-1.38356309103871E-16));
#15449=CARTESIAN_POINT('Origin',(0.,0.5,0.));
#15450=CARTESIAN_POINT('Origin',(0.,0.47,0.));
#15451=CARTESIAN_POINT('',(-1.6,0.44,-1.95943487863577E-16));
#15452=CARTESIAN_POINT('Origin',(0.,0.44,0.));
#15453=CARTESIAN_POINT('',(-1.57,0.47,-1.92269547466134E-16));
#15454=CARTESIAN_POINT('Origin',(0.,0.,0.));
#15455=CARTESIAN_POINT('',(-1.6,-0.44,-1.95943487863577E-16));
#15456=CARTESIAN_POINT('Origin',(0.,-0.44,0.));
#15457=CARTESIAN_POINT('',(-1.6,0.,-1.95943487863577E-16));
#15458=CARTESIAN_POINT('Origin',(0.,-0.47,0.));
#15459=CARTESIAN_POINT('',(-1.54,-0.5,-1.88595607068692E-16));
#15460=CARTESIAN_POINT('Origin',(0.,-0.5,0.));
#15461=CARTESIAN_POINT('',(-1.57,-0.47,-1.92269547466134E-16));
#15462=CARTESIAN_POINT('Origin',(1.129765,-0.5,0.));
#15463=CARTESIAN_POINT('Origin',(0.,0.,0.));
#15464=CARTESIAN_POINT('',(-1.129765,0.,-1.38356309103871E-16));
#15465=CARTESIAN_POINT('',(0.,0.,0.));
#15466=CARTESIAN_POINT('Origin',(1.1,0.,0.));
#15467=CARTESIAN_POINT('',(1.1,-2.23201749654651E-33,0.29765));
#15468=CARTESIAN_POINT('',(1.1,-2.23201749654651E-33,-0.29765));
#15469=CARTESIAN_POINT('Origin',(1.1,0.,0.));
#15470=CARTESIAN_POINT('Origin',(0.685838782044607,0.,-0.860014630714833));
#15471=CARTESIAN_POINT('',(0.918550922801216,-5.31350540756609E-33,-0.674432891191581));
#15472=CARTESIAN_POINT('',(0.453126641287998,8.49470414473068E-34,-1.04559637023808));
#15473=CARTESIAN_POINT('Origin',(0.685838782044607,0.,-0.860014630714833));
#15474=CARTESIAN_POINT('Origin',(-0.244773027351946,0.,-1.07242070340001));
#15475=CARTESIAN_POINT('',(0.0454142657089739,-2.23201749654651E-33,-1.1386540593921));
#15476=CARTESIAN_POINT('',(-0.534960320412865,-2.23201749654651E-33,-1.00618734740791));
#15477=CARTESIAN_POINT('Origin',(-0.244773027351946,0.,-1.07242070340001));
#15478=CARTESIAN_POINT('Origin',(-0.991065754692661,0.,-0.477272113029314));
#15479=CARTESIAN_POINT('',(-0.86192025974432,8.49470414473067E-34,-0.745445496560469));
#15480=CARTESIAN_POINT('',(-1.120211249641,-5.31350540756609E-33,-0.209098729498159));
#15481=CARTESIAN_POINT('Origin',(-0.991065754692661,0.,-0.477272113029314));
#15482=CARTESIAN_POINT('Origin',(-0.991065754692661,0.,0.477272113029314));
#15483=CARTESIAN_POINT('',(-1.120211249641,-2.23201749654651E-33,0.209098729498159));
#15484=CARTESIAN_POINT('',(-0.86192025974432,-2.23201749654651E-33,0.745445496560469));
#15485=CARTESIAN_POINT('Origin',(-0.991065754692661,0.,0.477272113029314));
#15486=CARTESIAN_POINT('Origin',(-0.244773027351946,0.,1.07242070340001));
#15487=CARTESIAN_POINT('',(-0.534960320412866,-2.23201749654651E-33,1.00618734740791));
#15488=CARTESIAN_POINT('',(0.0454142657089737,-2.23201749654651E-33,1.1386540593921));
#15489=CARTESIAN_POINT('Origin',(-0.244773027351946,0.,1.07242070340001));
#15490=CARTESIAN_POINT('Origin',(0.685838782044607,0.,0.860014630714833));
#15491=CARTESIAN_POINT('',(0.453126641287998,-2.23201749654651E-33,1.04559637023808));
#15492=CARTESIAN_POINT('',(0.918550922801216,-2.23201749654651E-33,0.674432891191581));
#15493=CARTESIAN_POINT('Origin',(0.685838782044607,0.,0.860014630714833));
#15494=CARTESIAN_POINT('',(0.,0.,0.));
#15495=CARTESIAN_POINT('Origin',(0.685838782044607,0.,0.860014630714833));
#15496=CARTESIAN_POINT('',(0.413083465285518,-0.05953,0.993751811093549));
#15497=CARTESIAN_POINT('',(0.876916659919095,-0.05953,0.623857181492959));
#15498=CARTESIAN_POINT('Ctrl Pts',(0.413083465285518,-0.05953,0.993751811093549));
#15499=CARTESIAN_POINT('Ctrl Pts',(0.419070565453383,-0.0925528133349865,
0.991263089003441));
#15500=CARTESIAN_POINT('Ctrl Pts',(0.430199341854858,-0.124911173756694,
0.986608710139579));
#15501=CARTESIAN_POINT('Ctrl Pts',(0.457978755888596,-0.177924977804098,
0.973971221090534));
#15502=CARTESIAN_POINT('Ctrl Pts',(0.473077587363685,-0.199697230012983,
0.966820759530997));
#15503=CARTESIAN_POINT('Ctrl Pts',(0.507057380724533,-0.237895043532788,
0.949440676105255));
#15504=CARTESIAN_POINT('Ctrl Pts',(0.525933334162555,-0.254319232363049,
0.939198248544428));
#15505=CARTESIAN_POINT('Ctrl Pts',(0.564362943424238,-0.28018331644634,
0.916597376014514));
#15506=CARTESIAN_POINT('Ctrl Pts',(0.585840553788742,-0.29104845371857,
0.903141581680914));
#15507=CARTESIAN_POINT('Ctrl Pts',(0.629305439856167,-0.30527573347708,
0.873412008702649));
#15508=CARTESIAN_POINT('Ctrl Pts',(0.651278921914856,-0.308638795020976,
0.857118508332695));
#15509=CARTESIAN_POINT('Ctrl Pts',(0.690705563850638,-0.308638795020976,
0.825676810575914));
#15510=CARTESIAN_POINT('Ctrl Pts',(0.711480111898423,-0.30527573347708,
0.807879894508811));
#15511=CARTESIAN_POINT('Ctrl Pts',(0.750136149454208,-0.29104845371857,
0.772120216227122));
#15512=CARTESIAN_POINT('Ctrl Pts',(0.768033796848072,-0.28018331644634,
0.754175290318038));
#15513=CARTESIAN_POINT('Ctrl Pts',(0.798619410861634,-0.254319232363049,
0.721738358858166));
#15514=CARTESIAN_POINT('Ctrl Pts',(0.812805334167529,-0.237895043532788,
0.705614819529209));
#15515=CARTESIAN_POINT('Ctrl Pts',(0.837310877969633,-0.199697230012983,
0.676354402927683));
#15516=CARTESIAN_POINT('Ctrl Pts',(0.847641868610495,-0.177924977804098,
0.663225258065736));
#15517=CARTESIAN_POINT('Ctrl Pts',(0.866144010579847,-0.124911173756694,
0.638954437806245));
#15518=CARTESIAN_POINT('Ctrl Pts',(0.873158080166742,-0.0925528133349865,
0.62914037979579));
#15519=CARTESIAN_POINT('Ctrl Pts',(0.876916659919095,-0.05953,0.623857181492959));
#15520=CARTESIAN_POINT('',(0.437601487681057,-0.05953,1.03511272300331));
#15521=CARTESIAN_POINT('Origin',(0.685838782044607,-0.05953,0.860014630714833));
#15522=CARTESIAN_POINT('',(0.911784794170997,-0.05953,0.656964154625313));
#15523=CARTESIAN_POINT('Ctrl Pts',(0.911784794170998,-0.0595300000000001,
0.656964154625312));
#15524=CARTESIAN_POINT('Ctrl Pts',(0.909827729890942,-0.0762225747374255,
0.659680317203144));
#15525=CARTESIAN_POINT('Ctrl Pts',(0.907004864562642,-0.0928409665394228,
0.663576540841106));
#15526=CARTESIAN_POINT('Ctrl Pts',(0.895234408667242,-0.144299303100741,
0.679480524217551));
#15527=CARTESIAN_POINT('Ctrl Pts',(0.882797231409153,-0.177024326825049,
0.695831250979106));
#15528=CARTESIAN_POINT('Ctrl Pts',(0.854332839576145,-0.227269801620064,
0.73042219438957));
#15529=CARTESIAN_POINT('Ctrl Pts',(0.834863020612702,-0.251265615809407,
0.752807465209441));
#15530=CARTESIAN_POINT('Ctrl Pts',(0.800439809856111,-0.279889827963178,
0.789147407129766));
#15531=CARTESIAN_POINT('Ctrl Pts',(0.781998747691871,-0.290879136862659,
0.80756613568454));
#15532=CARTESIAN_POINT('Ctrl Pts',(0.742239891936898,-0.305251990234487,
0.844254137480382));
#15533=CARTESIAN_POINT('Ctrl Pts',(0.720906778729541,-0.308638795020976,
0.862505527716294));
#15534=CARTESIAN_POINT('Ctrl Pts',(0.680463863683392,-0.308638795020976,
0.894757676234429));
#15535=CARTESIAN_POINT('Ctrl Pts',(0.657923009631182,-0.305251990234488,
0.91149460735272));
#15536=CARTESIAN_POINT('Ctrl Pts',(0.613307674922609,-0.290879136862659,
0.942092777160053));
#15537=CARTESIAN_POINT('Ctrl Pts',(0.591247219971725,-0.279889827963178,
0.955972930713954));
#15538=CARTESIAN_POINT('Ctrl Pts',(0.548158511259202,-0.251265615809407,
0.981446681891443));
#15539=CARTESIAN_POINT('Ctrl Pts',(0.522002043615455,-0.227269801620063,
0.995447160474328));
#15540=CARTESIAN_POINT('Ctrl Pts',(0.481944444320713,-0.177024326825049,
1.01550068154148));
#15541=CARTESIAN_POINT('Ctrl Pts',(0.463236132117164,-0.14429930310074,
1.0239876538093));
#15542=CARTESIAN_POINT('Ctrl Pts',(0.445111721969657,-0.0928409665394226,
1.03192403056628));
#15543=CARTESIAN_POINT('Ctrl Pts',(0.440685038163619,-0.0762225747374254,
1.03380912944435));
#15544=CARTESIAN_POINT('Ctrl Pts',(0.437601487681056,-0.05953,1.03511272300331));
#15545=CARTESIAN_POINT('Origin',(0.685838782044607,-0.05953,0.860014630714833));
#15546=CARTESIAN_POINT('Origin',(0.,-0.208355,0.));
#15547=CARTESIAN_POINT('',(0.0548532617164168,-0.05953,1.12247250791415));
#15548=CARTESIAN_POINT('Origin',(0.,-0.05953,0.));
#15549=CARTESIAN_POINT('',(-0.536443649899848,-0.05953,0.987512846410683));
#15550=CARTESIAN_POINT('Ctrl Pts',(0.0548532617164173,-0.0595300000000001,
1.12247250791414));
#15551=CARTESIAN_POINT('Ctrl Pts',(0.05150947068137,-0.0762225747374254,
1.12263591311425));
#15552=CARTESIAN_POINT('Ctrl Pts',(0.0467032526342597,-0.0928409665394227,
1.12285816383385));
#15553=CARTESIAN_POINT('Ctrl Pts',(0.0269302585198975,-0.144299303100741,
1.12357162229597));
#15554=CARTESIAN_POINT('Ctrl Pts',(0.006392292392153,-0.177024326825049,
1.12404235695137));
#15555=CARTESIAN_POINT('Ctrl Pts',(-0.0383992541984087,-0.227269801620063,
1.12335509974011));
#15556=CARTESIAN_POINT('Ctrl Pts',(-0.0680399972366993,-0.251265615809407,
1.12208997038458));
#15557=CARTESIAN_POINT('Ctrl Pts',(-0.117914228755037,-0.279889827963178,
1.1178344036749));
#15558=CARTESIAN_POINT('Ctrl Pts',(-0.14381238480104,-0.290879136862659,
1.11490049012186));
#15559=CARTESIAN_POINT('Ctrl Pts',(-0.19728546073067,-0.305251990234488,
1.10669035995599));
#15560=CARTESIAN_POINT('Ctrl Pts',(-0.224855950742601,-0.308638795020976,
1.10139101611326));
#15561=CARTESIAN_POINT('Ctrl Pts',(-0.275287440920027,-0.308638795020976,
1.0898803575765));
#15562=CARTESIAN_POINT('Ctrl Pts',(-0.302426893214945,-0.305251990234488,
1.08269251410343));
#15563=CARTESIAN_POINT('Ctrl Pts',(-0.35416671187353,-0.290879136862659,
1.06688848765783));
#15564=CARTESIAN_POINT('Ctrl Pts',(-0.3787731215897,-0.279889827963178,
1.05829506364875));
#15565=CARTESIAN_POINT('Ctrl Pts',(-0.425554672694338,-0.251265615809407,
1.04048957871266));
#15566=CARTESIAN_POINT('Ctrl Pts',(-0.452808978448581,-0.227269801620063,
1.02876878445619));
#15567=CARTESIAN_POINT('Ctrl Pts',(-0.493462957200432,-0.177024326825049,
1.0099536580922));
#15568=CARTESIAN_POINT('Ctrl Pts',(-0.511762781179148,-0.14429930310074,
1.00061845128527));
#15569=CARTESIAN_POINT('Ctrl Pts',(-0.529268075276157,-0.0928409665394226,
0.991396466802468));
#15570=CARTESIAN_POINT('Ctrl Pts',(-0.533501897135713,-0.0762225747374254,
0.989110885965947));
#15571=CARTESIAN_POINT('Ctrl Pts',(-0.536443649899848,-0.0595300000000001,
0.987512846410683));
#15572=CARTESIAN_POINT('',(-0.843383895613249,-0.05953,0.742736168477219));
#15573=CARTESIAN_POINT('Origin',(0.,-0.05953,0.));
#15574=CARTESIAN_POINT('',(-1.10653577764992,-0.05953,0.196295654879792));
#15575=CARTESIAN_POINT('Ctrl Pts',(-0.843383895613249,-0.0595300000000001,
0.742736168477219));
#15576=CARTESIAN_POINT('Ctrl Pts',(-0.84559647055299,-0.0762225747374255,
0.740223768851062));
#15577=CARTESIAN_POINT('Ctrl Pts',(-0.848766861100456,-0.0928409665394227,
0.736604687327351));
#15578=CARTESIAN_POINT('Ctrl Pts',(-0.861652925570091,-0.144299303100741,
0.721590372101268));
#15579=CARTESIAN_POINT('Ctrl Pts',(-0.87482617317514,-0.177024326825049,
0.705826641853758));
#15580=CARTESIAN_POINT('Ctrl Pts',(-0.902215926359523,-0.227269801620063,
0.670378702718353));
#15581=CARTESIAN_POINT('Ctrl Pts',(-0.919707509403859,-0.251265615809407,
0.646415841396062));
#15582=CARTESIAN_POINT('Ctrl Pts',(-0.947476448101718,-0.279889827963178,
0.604769294586516));
#15583=CARTESIAN_POINT('Ctrl Pts',(-0.961329858300736,-0.290879136862659,
0.582692035672022));
#15584=CARTESIAN_POINT('Ctrl Pts',(-0.988250837578047,-0.305251990234488,
0.535766169015486));
#15585=CARTESIAN_POINT('Ctrl Pts',(-1.00129756308006,-0.308638795020976,
0.510906605094603));
#15586=CARTESIAN_POINT('Ctrl Pts',(-1.02374168767024,-0.308638795020976,
0.46430090015576));
#15587=CARTESIAN_POINT('Ctrl Pts',(-1.03504317708586,-0.305251990234488,
0.438600874831839));
#15588=CARTESIAN_POINT('Ctrl Pts',(-1.05494634094458,-0.290879136862659,
0.388295406390235));
#15589=CARTESIAN_POINT('Ctrl Pts',(-1.06356957703048,-0.279889827963178,
0.363699428370917));
#15590=CARTESIAN_POINT('Ctrl Pts',(-1.0788165083757,-0.251265615809407,
0.316022600643821));
#15591=CARTESIAN_POINT('Ctrl Pts',(-1.08664560412098,-0.227269801620063,
0.287406530683752));
#15592=CARTESIAN_POINT('Ctrl Pts',(-1.09728268713976,-0.177024326825049,
0.243890930799337));
#15593=CARTESIAN_POINT('Ctrl Pts',(-1.10139388218929,-0.144299303100741,
0.22376314604679));
#15594=CARTESIAN_POINT('Ctrl Pts',(-1.10509821673782,-0.0928409665394227,
0.204327142733961));
#15595=CARTESIAN_POINT('Ctrl Pts',(-1.10595102243643,-0.0762225747374254,
0.199591971170104));
#15596=CARTESIAN_POINT('Ctrl Pts',(-1.10653577764992,-0.0595300000000001,
0.196295654879792));
#15597=CARTESIAN_POINT('',(-1.123812,-0.05953,1.37627276864339E-16));
#15598=CARTESIAN_POINT('Origin',(0.,-0.05953,0.));
#15599=CARTESIAN_POINT('',(-1.123812,-0.35718,1.37627276864339E-16));
#15600=CARTESIAN_POINT('',(-1.123812,-0.208355,1.37627276864339E-16));
#15601=CARTESIAN_POINT('Origin',(0.,-0.35718,0.));
#15602=CARTESIAN_POINT('',(-1.10653577764992,-0.05953,-0.196295654879793));
#15603=CARTESIAN_POINT('Origin',(0.,-0.05953,0.));
#15604=CARTESIAN_POINT('',(-0.843383895613249,-0.05953,-0.742736168477219));
#15605=CARTESIAN_POINT('Ctrl Pts',(-1.10653577764992,-0.0595300000000001,
-0.196295654879792));
#15606=CARTESIAN_POINT('Ctrl Pts',(-1.10595102243643,-0.0762225747374255,
-0.199591971170104));
#15607=CARTESIAN_POINT('Ctrl Pts',(-1.10509821673782,-0.0928409665394228,
-0.204327142733962));
#15608=CARTESIAN_POINT('Ctrl Pts',(-1.10139388218929,-0.144299303100741,
-0.22376314604679));
#15609=CARTESIAN_POINT('Ctrl Pts',(-1.09728268713976,-0.177024326825049,
-0.243890930799338));
#15610=CARTESIAN_POINT('Ctrl Pts',(-1.08664560412098,-0.227269801620063,
-0.287406530683753));
#15611=CARTESIAN_POINT('Ctrl Pts',(-1.0788165083757,-0.251265615809407,
-0.316022600643821));
#15612=CARTESIAN_POINT('Ctrl Pts',(-1.06356957703048,-0.279889827963178,
-0.363699428370918));
#15613=CARTESIAN_POINT('Ctrl Pts',(-1.05494634094458,-0.290879136862659,
-0.388295406390235));
#15614=CARTESIAN_POINT('Ctrl Pts',(-1.03504317708586,-0.305251990234488,
-0.438600874831839));
#15615=CARTESIAN_POINT('Ctrl Pts',(-1.02374168767024,-0.308638795020976,
-0.46430090015576));
#15616=CARTESIAN_POINT('Ctrl Pts',(-1.00129756308006,-0.308638795020976,
-0.510906605094603));
#15617=CARTESIAN_POINT('Ctrl Pts',(-0.988250837578047,-0.305251990234488,
-0.535766169015486));
#15618=CARTESIAN_POINT('Ctrl Pts',(-0.961329858300736,-0.290879136862659,
-0.582692035672022));
#15619=CARTESIAN_POINT('Ctrl Pts',(-0.947476448101718,-0.279889827963178,
-0.604769294586516));
#15620=CARTESIAN_POINT('Ctrl Pts',(-0.919707509403859,-0.251265615809407,
-0.646415841396062));
#15621=CARTESIAN_POINT('Ctrl Pts',(-0.902215926359523,-0.227269801620064,
-0.670378702718353));
#15622=CARTESIAN_POINT('Ctrl Pts',(-0.87482617317514,-0.177024326825049,
-0.705826641853758));
#15623=CARTESIAN_POINT('Ctrl Pts',(-0.861652925570091,-0.144299303100741,
-0.721590372101268));
#15624=CARTESIAN_POINT('Ctrl Pts',(-0.848766861100456,-0.0928409665394229,
-0.736604687327351));
#15625=CARTESIAN_POINT('Ctrl Pts',(-0.84559647055299,-0.0762225747374255,
-0.740223768851063));
#15626=CARTESIAN_POINT('Ctrl Pts',(-0.843383895613249,-0.0595300000000001,
-0.742736168477219));
#15627=CARTESIAN_POINT('',(-0.536443649899847,-0.05953,-0.987512846410683));
#15628=CARTESIAN_POINT('Origin',(0.,-0.05953,0.));
#15629=CARTESIAN_POINT('',(0.0548532617164172,-0.05953,-1.12247250791415));
#15630=CARTESIAN_POINT('Ctrl Pts',(-0.536443649899848,-0.0595300000000001,
-0.987512846410683));
#15631=CARTESIAN_POINT('Ctrl Pts',(-0.533501897135712,-0.0762225747374254,
-0.989110885965947));
#15632=CARTESIAN_POINT('Ctrl Pts',(-0.529268075276156,-0.0928409665394227,
-0.991396466802469));
#15633=CARTESIAN_POINT('Ctrl Pts',(-0.511762781179147,-0.144299303100741,
-1.00061845128527));
#15634=CARTESIAN_POINT('Ctrl Pts',(-0.493462957200432,-0.177024326825049,
-1.0099536580922));
#15635=CARTESIAN_POINT('Ctrl Pts',(-0.45280897844858,-0.227269801620063,
-1.02876878445619));
#15636=CARTESIAN_POINT('Ctrl Pts',(-0.425554672694337,-0.251265615809407,
-1.04048957871266));
#15637=CARTESIAN_POINT('Ctrl Pts',(-0.3787731215897,-0.279889827963178,
-1.05829506364875));
#15638=CARTESIAN_POINT('Ctrl Pts',(-0.354166711873529,-0.290879136862659,
-1.06688848765783));
#15639=CARTESIAN_POINT('Ctrl Pts',(-0.302426893214944,-0.305251990234488,
-1.08269251410343));
#15640=CARTESIAN_POINT('Ctrl Pts',(-0.275287440920027,-0.308638795020976,
-1.0898803575765));
#15641=CARTESIAN_POINT('Ctrl Pts',(-0.224855950742601,-0.308638795020976,
-1.10139101611326));
#15642=CARTESIAN_POINT('Ctrl Pts',(-0.19728546073067,-0.305251990234488,
-1.10669035995599));
#15643=CARTESIAN_POINT('Ctrl Pts',(-0.143812384801039,-0.290879136862659,
-1.11490049012186));
#15644=CARTESIAN_POINT('Ctrl Pts',(-0.117914228755037,-0.279889827963178,
-1.1178344036749));
#15645=CARTESIAN_POINT('Ctrl Pts',(-0.0680399972366989,-0.251265615809407,
-1.12208997038458));
#15646=CARTESIAN_POINT('Ctrl Pts',(-0.0383992541984084,-0.227269801620063,
-1.12335509974011));
#15647=CARTESIAN_POINT('Ctrl Pts',(0.00639229239215326,-0.177024326825049,
-1.12404235695137));
#15648=CARTESIAN_POINT('Ctrl Pts',(0.0269302585198977,-0.144299303100741,
-1.12357162229597));
#15649=CARTESIAN_POINT('Ctrl Pts',(0.04670325263426,-0.0928409665394228,
-1.12285816383385));
#15650=CARTESIAN_POINT('Ctrl Pts',(0.0515094706813703,-0.0762225747374255,
-1.12263591311425));
#15651=CARTESIAN_POINT('Ctrl Pts',(0.0548532617164176,-0.0595300000000001,
-1.12247250791414));
#15652=CARTESIAN_POINT('',(0.437601487681057,-0.05953,-1.03511272300331));
#15653=CARTESIAN_POINT('Origin',(0.,-0.05953,0.));
#15654=CARTESIAN_POINT('',(0.911784794170997,-0.05953,-0.656964154625313));
#15655=CARTESIAN_POINT('Ctrl Pts',(0.437601487681056,-0.0595300000000001,
-1.03511272300331));
#15656=CARTESIAN_POINT('Ctrl Pts',(0.440685038163619,-0.0762225747374255,
-1.03380912944435));
#15657=CARTESIAN_POINT('Ctrl Pts',(0.445111721969657,-0.0928409665394228,
-1.03192403056628));
#15658=CARTESIAN_POINT('Ctrl Pts',(0.463236132117164,-0.144299303100741,
-1.0239876538093));
#15659=CARTESIAN_POINT('Ctrl Pts',(0.481944444320713,-0.177024326825049,
-1.01550068154148));
#15660=CARTESIAN_POINT('Ctrl Pts',(0.522002043615455,-0.227269801620064,
-0.995447160474328));
#15661=CARTESIAN_POINT('Ctrl Pts',(0.548158511259203,-0.251265615809407,
-0.981446681891443));
#15662=CARTESIAN_POINT('Ctrl Pts',(0.591247219971725,-0.279889827963178,
-0.955972930713954));
#15663=CARTESIAN_POINT('Ctrl Pts',(0.613307674922609,-0.290879136862659,
-0.942092777160053));
#15664=CARTESIAN_POINT('Ctrl Pts',(0.657923009631182,-0.305251990234487,
-0.91149460735272));
#15665=CARTESIAN_POINT('Ctrl Pts',(0.680463863683393,-0.308638795020976,
-0.894757676234429));
#15666=CARTESIAN_POINT('Ctrl Pts',(0.720906778729542,-0.308638795020976,
-0.862505527716294));
#15667=CARTESIAN_POINT('Ctrl Pts',(0.742239891936899,-0.305251990234488,
-0.844254137480381));
#15668=CARTESIAN_POINT('Ctrl Pts',(0.781998747691872,-0.290879136862659,
-0.80756613568454));
#15669=CARTESIAN_POINT('Ctrl Pts',(0.800439809856112,-0.279889827963178,
-0.789147407129765));
#15670=CARTESIAN_POINT('Ctrl Pts',(0.834863020612702,-0.251265615809407,
-0.752807465209441));
#15671=CARTESIAN_POINT('Ctrl Pts',(0.854332839576145,-0.227269801620064,
-0.73042219438957));
#15672=CARTESIAN_POINT('Ctrl Pts',(0.882797231409153,-0.177024326825049,
-0.695831250979106));
#15673=CARTESIAN_POINT('Ctrl Pts',(0.895234408667242,-0.144299303100741,
-0.679480524217551));
#15674=CARTESIAN_POINT('Ctrl Pts',(0.907004864562642,-0.0928409665394228,
-0.663576540841106));
#15675=CARTESIAN_POINT('Ctrl Pts',(0.909827729890942,-0.0762225747374256,
-0.659680317203144));
#15676=CARTESIAN_POINT('Ctrl Pts',(0.911784794170998,-0.0595300000000001,
-0.656964154625312));
#15677=CARTESIAN_POINT('',(1.08212377959455,-0.05953,-0.303251606722892));
#15678=CARTESIAN_POINT('Origin',(0.,-0.05953,0.));
#15679=CARTESIAN_POINT('',(1.08212377959455,-0.05953,0.303251606722892));
#15680=CARTESIAN_POINT('Ctrl Pts',(1.08212377959455,-0.0595300000000001,
-0.303251606722892));
#15681=CARTESIAN_POINT('Ctrl Pts',(1.0830271513892,-0.0762225747374255,
-0.300028012588062));
#15682=CARTESIAN_POINT('Ctrl Pts',(1.08431331394788,-0.0928409665394228,
-0.2953917518996));
#15683=CARTESIAN_POINT('Ctrl Pts',(1.08940878963422,-0.144299303100741,
-0.276273267473431));
#15684=CARTESIAN_POINT('Ctrl Pts',(1.09443784939331,-0.177024326825049,
-0.256354979351213));
#15685=CARTESIAN_POINT('Ctrl Pts',(1.10373487993589,-0.227269801620064,
-0.212533521233765));
#15686=CARTESIAN_POINT('Ctrl Pts',(1.10909715583869,-0.251265615809407,
-0.183354415742157));
#15687=CARTESIAN_POINT('Ctrl Pts',(1.1160463456491,-0.279889827963178,-0.133783682657561));
#15688=CARTESIAN_POINT('Ctrl Pts',(1.11894887330541,-0.290879136862659,
-0.107881990270302));
#15689=CARTESIAN_POINT('Ctrl Pts',(1.12284346704144,-0.305251990234488,
-0.0539226701638766));
#15690=CARTESIAN_POINT('Ctrl Pts',(1.123812,-0.308638795020976,-0.025864214957475));
#15691=CARTESIAN_POINT('Ctrl Pts',(1.123812,-0.308638795020976,0.025864214957475));
#15692=CARTESIAN_POINT('Ctrl Pts',(1.12284346704144,-0.305251990234488,
0.0539226701638766));
#15693=CARTESIAN_POINT('Ctrl Pts',(1.11894887330541,-0.290879136862659,
0.107881990270302));
#15694=CARTESIAN_POINT('Ctrl Pts',(1.1160463456491,-0.279889827963178,0.133783682657561));
#15695=CARTESIAN_POINT('Ctrl Pts',(1.10909715583869,-0.251265615809407,
0.183354415742157));
#15696=CARTESIAN_POINT('Ctrl Pts',(1.10373487993589,-0.227269801620064,
0.212533521233765));
#15697=CARTESIAN_POINT('Ctrl Pts',(1.09443784939331,-0.177024326825049,
0.256354979351213));
#15698=CARTESIAN_POINT('Ctrl Pts',(1.08940878963422,-0.144299303100741,
0.276273267473431));
#15699=CARTESIAN_POINT('Ctrl Pts',(1.08431331394788,-0.0928409665394228,
0.2953917518996));
#15700=CARTESIAN_POINT('Ctrl Pts',(1.0830271513892,-0.0762225747374255,
0.300028012588062));
#15701=CARTESIAN_POINT('Ctrl Pts',(1.08212377959455,-0.0595300000000001,
0.303251606722892));
#15702=CARTESIAN_POINT('Origin',(0.,-0.05953,0.));
#15703=CARTESIAN_POINT('Origin',(0.,-0.05953,0.));
#15704=CARTESIAN_POINT('',(0.0589974094846122,-0.05953,1.07456964270265));
#15705=CARTESIAN_POINT('Origin',(0.,-0.05953,0.));
#15706=CARTESIAN_POINT('Origin',(-0.244773027351946,-0.05953,1.07242070340001));
#15707=CARTESIAN_POINT('Origin',(-0.244773027351946,0.,1.07242070340001));
#15708=CARTESIAN_POINT('',(-0.519393123750572,-0.05953,0.942555777842682));
#15709=CARTESIAN_POINT('Ctrl Pts',(-0.519393123750572,-0.05953,0.942555777842682));
#15710=CARTESIAN_POINT('Ctrl Pts',(-0.513714466572041,-0.0925528133349865,
0.945684988399766));
#15711=CARTESIAN_POINT('Ctrl Pts',(-0.503136848051455,-0.124911173756694,
0.951483858396181));
#15712=CARTESIAN_POINT('Ctrl Pts',(-0.47593627990192,-0.177924977804098,
0.965323333309091));
#15713=CARTESIAN_POINT('Ctrl Pts',(-0.460931856495794,-0.199697230012983,
0.972669835243841));
#15714=CARTESIAN_POINT('Ctrl Pts',(-0.426157505475872,-0.237895043532788,
0.988400002689705));
#15715=CARTESIAN_POINT('Ctrl Pts',(-0.406380688682952,-0.254319232363049,
0.996771768218699));
#15716=CARTESIAN_POINT('Ctrl Pts',(-0.364750145543744,-0.28018331644634,
1.01272583306292));
#15717=CARTESIAN_POINT('Ctrl Pts',(-0.340838910881557,-0.29104845371857,
1.02112815447116));
#15718=CARTESIAN_POINT('Ctrl Pts',(-0.290495481564827,-0.30527573347708,
1.036574285215));
#15719=CARTESIAN_POINT('Ctrl Pts',(-0.264056468041074,-0.308638795020976,
1.04359501395068));
#15720=CARTESIAN_POINT('Ctrl Pts',(-0.214892249704082,-0.308638795020976,
1.05481642595959));
#15721=CARTESIAN_POINT('Ctrl Pts',(-0.188025341585962,-0.30527573347708,
1.05996242598502));
#15722=CARTESIAN_POINT('Ctrl Pts',(-0.135965654106109,-0.29104845371857,
1.06788913840721));
#15723=CARTESIAN_POINT('Ctrl Pts',(-0.110776745452494,-0.28018331644634,
1.07069360430242));
#15724=CARTESIAN_POINT('Ctrl Pts',(-0.0663467128214646,-0.254319232363049,
1.07438230428002));
#15725=CARTESIAN_POINT('Ctrl Pts',(-0.0448960436540983,-0.237895043532788,
1.07542044338697));
#15726=CARTESIAN_POINT('Ctrl Pts',(-0.00674037211528124,-0.199697230012983,
1.07633607767727));
#15727=CARTESIAN_POINT('Ctrl Pts',(0.00996567398334777,-0.177924977804098,
1.07622728347683));
#15728=CARTESIAN_POINT('Ctrl Pts',(0.0404772621979741,-0.124911173756694,
1.07556023164702));
#15729=CARTESIAN_POINT('Ctrl Pts',(0.0525234025782719,-0.0925528133349865,
1.07492508698591));
#15730=CARTESIAN_POINT('Ctrl Pts',(0.0589974094846124,-0.05953,1.07456964270265));
#15731=CARTESIAN_POINT('Origin',(-0.244773027351946,-0.05953,1.07242070340001));
#15732=CARTESIAN_POINT('Origin',(0.,-0.05953,0.));
#15733=CARTESIAN_POINT('',(-0.803348093619616,-0.05953,0.716109245731214));
#15734=CARTESIAN_POINT('Origin',(0.,-0.05953,0.));
#15735=CARTESIAN_POINT('Origin',(-0.991065754692661,-0.05953,0.477272113029314));
#15736=CARTESIAN_POINT('Origin',(-0.991065754692661,0.,0.477272113029314));
#15737=CARTESIAN_POINT('',(-1.06075609691358,-0.05953,0.181596019242328));
#15738=CARTESIAN_POINT('Ctrl Pts',(-1.06075609691358,-0.05953,0.181596019242328));
#15739=CARTESIAN_POINT('Ctrl Pts',(-1.05966202740332,-0.0925528133349865,
0.187986803072856));
#15740=CARTESIAN_POINT('Ctrl Pts',(-1.05760072925372,-0.124911173756694,
0.199872254546857));
#15741=CARTESIAN_POINT('Ctrl Pts',(-1.05146158959546,-0.177924977804098,
0.22976728653846));
#15742=CARTESIAN_POINT('Ctrl Pts',(-1.04785021111757,-0.199697230012983,
0.246078686169301));
#15743=CARTESIAN_POINT('Ctrl Pts',(-1.03846709802406,-0.237895043532788,
0.283073967563097));
#15744=CARTESIAN_POINT('Ctrl Pts',(-1.03268176429485,-0.254319232363049,
0.303755815985685));
#15745=CARTESIAN_POINT('Ctrl Pts',(-1.01919893537026,-0.28018331644634,
0.346251081972725));
#15746=CARTESIAN_POINT('Ctrl Pts',(-1.01085972381132,-0.29104845371857,
0.370184399726282));
#15747=CARTESIAN_POINT('Ctrl Pts',(-0.99154738033959,-0.30527573347708,
0.419174982698463));
#15748=CARTESIAN_POINT('Ctrl Pts',(-0.980551951791748,-0.308638795020976,
0.444223188605045));
#15749=CARTESIAN_POINT('Ctrl Pts',(-0.958671816228589,-0.308638795020976,
0.489657758261848));
#15750=CARTESIAN_POINT('Ctrl Pts',(-0.945943877838127,-0.30527573347708,
0.51387163140139));
#15751=CARTESIAN_POINT('Ctrl Pts',(-0.91968254693063,-0.29104845371857,
0.559515758398093));
#15752=CARTESIAN_POINT('Ctrl Pts',(-0.906170138993533,-0.28018331644634,
0.580957796077825));
#15753=CARTESIAN_POINT('Ctrl Pts',(-0.8813524085237,-0.254319232363049,
0.617994461173994));
#15754=CARTESIAN_POINT('Ctrl Pts',(-0.868789784891799,-0.237895043532788,
0.635412538795143));
#15755=CARTESIAN_POINT('Ctrl Pts',(-0.845715984518854,-0.199697230012983,
0.66581473268113));
#15756=CARTESIAN_POINT('Ctrl Pts',(-0.835214876415962,-0.177924977804098,
0.678808213394124));
#15757=CARTESIAN_POINT('Ctrl Pts',(-0.815669690204649,-0.124911173756694,
0.702247233627224));
#15758=CARTESIAN_POINT('Ctrl Pts',(-0.807662468433796,-0.0925528133349865,
0.711269279199861));
#15759=CARTESIAN_POINT('Ctrl Pts',(-0.803348093619616,-0.05953,0.716109245731214));
#15760=CARTESIAN_POINT('Origin',(-0.991065754692661,-0.05953,0.477272113029314));
#15761=CARTESIAN_POINT('Origin',(0.,-0.05953,0.));
#15762=CARTESIAN_POINT('',(-1.076188,-0.05953,1.31795018948079E-16));
#15763=CARTESIAN_POINT('Origin',(0.,-0.05953,0.));
#15764=CARTESIAN_POINT('',(-1.06075609691358,-0.05953,-0.181596019242328));
#15765=CARTESIAN_POINT('Origin',(0.,-0.05953,0.));
#15766=CARTESIAN_POINT('Origin',(-0.991065754692661,-0.05953,-0.477272113029314));
#15767=CARTESIAN_POINT('Origin',(-0.991065754692661,0.,-0.477272113029314));
#15768=CARTESIAN_POINT('',(-0.803348093619616,-0.05953,-0.716109245731215));
#15769=CARTESIAN_POINT('Ctrl Pts',(-0.803348093619616,-0.05953,-0.716109245731215));
#15770=CARTESIAN_POINT('Ctrl Pts',(-0.807662468433795,-0.0925528133349865,
-0.711269279199862));
#15771=CARTESIAN_POINT('Ctrl Pts',(-0.815669690204649,-0.124911173756694,
-0.702247233627224));
#15772=CARTESIAN_POINT('Ctrl Pts',(-0.835214876415962,-0.177924977804098,
-0.678808213394124));
#15773=CARTESIAN_POINT('Ctrl Pts',(-0.845715984518854,-0.199697230012983,
-0.66581473268113));
#15774=CARTESIAN_POINT('Ctrl Pts',(-0.868789784891799,-0.237895043532788,
-0.635412538795143));
#15775=CARTESIAN_POINT('Ctrl Pts',(-0.8813524085237,-0.254319232363049,
-0.617994461173994));
#15776=CARTESIAN_POINT('Ctrl Pts',(-0.906170138993533,-0.28018331644634,
-0.580957796077826));
#15777=CARTESIAN_POINT('Ctrl Pts',(-0.91968254693063,-0.29104845371857,
-0.559515758398093));
#15778=CARTESIAN_POINT('Ctrl Pts',(-0.945943877838127,-0.30527573347708,
-0.51387163140139));
#15779=CARTESIAN_POINT('Ctrl Pts',(-0.958671816228589,-0.308638795020976,
-0.489657758261848));
#15780=CARTESIAN_POINT('Ctrl Pts',(-0.980551951791748,-0.308638795020976,
-0.444223188605045));
#15781=CARTESIAN_POINT('Ctrl Pts',(-0.99154738033959,-0.30527573347708,
-0.419174982698463));
#15782=CARTESIAN_POINT('Ctrl Pts',(-1.01085972381132,-0.29104845371857,
-0.370184399726282));
#15783=CARTESIAN_POINT('Ctrl Pts',(-1.01919893537026,-0.28018331644634,
-0.346251081972725));
#15784=CARTESIAN_POINT('Ctrl Pts',(-1.03268176429485,-0.254319232363049,
-0.303755815985685));
#15785=CARTESIAN_POINT('Ctrl Pts',(-1.03846709802406,-0.237895043532788,
-0.283073967563097));
#15786=CARTESIAN_POINT('Ctrl Pts',(-1.04785021111757,-0.199697230012983,
-0.246078686169302));
#15787=CARTESIAN_POINT('Ctrl Pts',(-1.05146158959546,-0.177924977804098,
-0.229767286538461));
#15788=CARTESIAN_POINT('Ctrl Pts',(-1.05760072925372,-0.124911173756694,
-0.199872254546858));
#15789=CARTESIAN_POINT('Ctrl Pts',(-1.05966202740332,-0.0925528133349864,
-0.187986803072857));
#15790=CARTESIAN_POINT('Ctrl Pts',(-1.06075609691358,-0.05953,-0.181596019242328));
#15791=CARTESIAN_POINT('Origin',(-0.991065754692661,-0.05953,-0.477272113029314));
#15792=CARTESIAN_POINT('Origin',(0.,-0.05953,0.));
#15793=CARTESIAN_POINT('',(-0.519393123750572,-0.05953,-0.942555777842682));
#15794=CARTESIAN_POINT('Origin',(0.,-0.05953,0.));
#15795=CARTESIAN_POINT('Origin',(-0.244773027351946,-0.05953,-1.07242070340001));
#15796=CARTESIAN_POINT('Origin',(-0.244773027351946,0.,-1.07242070340001));
#15797=CARTESIAN_POINT('',(0.0589974094846125,-0.05953,-1.07456964270265));
#15798=CARTESIAN_POINT('Ctrl Pts',(0.0589974094846127,-0.05953,-1.07456964270265));
#15799=CARTESIAN_POINT('Ctrl Pts',(0.0525234025782722,-0.0925528133349865,
-1.07492508698591));
#15800=CARTESIAN_POINT('Ctrl Pts',(0.0404772621979744,-0.124911173756694,
-1.07556023164702));
#15801=CARTESIAN_POINT('Ctrl Pts',(0.0099656739833481,-0.177924977804098,
-1.07622728347683));
#15802=CARTESIAN_POINT('Ctrl Pts',(-0.00674037211528096,-0.199697230012983,
-1.07633607767727));
#15803=CARTESIAN_POINT('Ctrl Pts',(-0.044896043654098,-0.237895043532788,
-1.07542044338697));
#15804=CARTESIAN_POINT('Ctrl Pts',(-0.0663467128214644,-0.254319232363049,
-1.07438230428002));
#15805=CARTESIAN_POINT('Ctrl Pts',(-0.110776745452493,-0.28018331644634,
-1.07069360430242));
#15806=CARTESIAN_POINT('Ctrl Pts',(-0.135965654106109,-0.29104845371857,
-1.06788913840721));
#15807=CARTESIAN_POINT('Ctrl Pts',(-0.188025341585962,-0.30527573347708,
-1.05996242598502));
#15808=CARTESIAN_POINT('Ctrl Pts',(-0.214892249704082,-0.308638795020976,
-1.05481642595959));
#15809=CARTESIAN_POINT('Ctrl Pts',(-0.264056468041074,-0.308638795020976,
-1.04359501395068));
#15810=CARTESIAN_POINT('Ctrl Pts',(-0.290495481564827,-0.30527573347708,
-1.036574285215));
#15811=CARTESIAN_POINT('Ctrl Pts',(-0.340838910881557,-0.291048453718569,
-1.02112815447116));
#15812=CARTESIAN_POINT('Ctrl Pts',(-0.364750145543744,-0.28018331644634,
-1.01272583306292));
#15813=CARTESIAN_POINT('Ctrl Pts',(-0.406380688682952,-0.254319232363049,
-0.996771768218699));
#15814=CARTESIAN_POINT('Ctrl Pts',(-0.426157505475872,-0.237895043532788,
-0.988400002689705));
#15815=CARTESIAN_POINT('Ctrl Pts',(-0.460931856495794,-0.199697230012983,
-0.972669835243841));
#15816=CARTESIAN_POINT('Ctrl Pts',(-0.475936279901919,-0.177924977804098,
-0.965323333309091));
#15817=CARTESIAN_POINT('Ctrl Pts',(-0.503136848051454,-0.124911173756694,
-0.951483858396181));
#15818=CARTESIAN_POINT('Ctrl Pts',(-0.513714466572041,-0.0925528133349865,
-0.945684988399766));
#15819=CARTESIAN_POINT('Ctrl Pts',(-0.519393123750572,-0.05953,-0.942555777842682));
#15820=CARTESIAN_POINT('Origin',(-0.244773027351946,-0.05953,-1.07242070340001));
#15821=CARTESIAN_POINT('Origin',(0.,-0.05953,0.));
#15822=CARTESIAN_POINT('',(0.413083465285518,-0.05953,-0.993751811093549));
#15823=CARTESIAN_POINT('Origin',(0.,-0.05953,0.));
#15824=CARTESIAN_POINT('Origin',(0.685838782044607,-0.05953,-0.860014630714833));
#15825=CARTESIAN_POINT('Origin',(0.685838782044607,0.,-0.860014630714833));
#15826=CARTESIAN_POINT('',(0.876916659919095,-0.05953,-0.623857181492959));
#15827=CARTESIAN_POINT('Ctrl Pts',(0.876916659919095,-0.05953,-0.623857181492958));
#15828=CARTESIAN_POINT('Ctrl Pts',(0.873158080166742,-0.0925528133349865,
-0.62914037979579));
#15829=CARTESIAN_POINT('Ctrl Pts',(0.866144010579847,-0.124911173756694,
-0.638954437806245));
#15830=CARTESIAN_POINT('Ctrl Pts',(0.847641868610495,-0.177924977804098,
-0.663225258065736));
#15831=CARTESIAN_POINT('Ctrl Pts',(0.837310877969633,-0.199697230012983,
-0.676354402927683));
#15832=CARTESIAN_POINT('Ctrl Pts',(0.81280533416753,-0.237895043532788,
-0.705614819529209));
#15833=CARTESIAN_POINT('Ctrl Pts',(0.798619410861634,-0.254319232363049,
-0.721738358858166));
#15834=CARTESIAN_POINT('Ctrl Pts',(0.768033796848072,-0.28018331644634,
-0.754175290318038));
#15835=CARTESIAN_POINT('Ctrl Pts',(0.750136149454208,-0.29104845371857,
-0.772120216227122));
#15836=CARTESIAN_POINT('Ctrl Pts',(0.711480111898423,-0.30527573347708,
-0.807879894508811));
#15837=CARTESIAN_POINT('Ctrl Pts',(0.690705563850638,-0.308638795020976,
-0.825676810575913));
#15838=CARTESIAN_POINT('Ctrl Pts',(0.651278921914856,-0.308638795020976,
-0.857118508332695));
#15839=CARTESIAN_POINT('Ctrl Pts',(0.629305439856167,-0.30527573347708,
-0.873412008702649));
#15840=CARTESIAN_POINT('Ctrl Pts',(0.585840553788742,-0.29104845371857,
-0.903141581680914));
#15841=CARTESIAN_POINT('Ctrl Pts',(0.564362943424239,-0.28018331644634,
-0.916597376014514));
#15842=CARTESIAN_POINT('Ctrl Pts',(0.525933334162556,-0.254319232363049,
-0.939198248544427));
#15843=CARTESIAN_POINT('Ctrl Pts',(0.507057380724533,-0.237895043532788,
-0.949440676105255));
#15844=CARTESIAN_POINT('Ctrl Pts',(0.473077587363686,-0.199697230012983,
-0.966820759530997));
#15845=CARTESIAN_POINT('Ctrl Pts',(0.457978755888596,-0.177924977804098,
-0.973971221090534));
#15846=CARTESIAN_POINT('Ctrl Pts',(0.430199341854858,-0.124911173756694,
-0.986608710139579));
#15847=CARTESIAN_POINT('Ctrl Pts',(0.419070565453384,-0.0925528133349865,
-0.991263089003441));
#15848=CARTESIAN_POINT('Ctrl Pts',(0.413083465285518,-0.05953,-0.993751811093549));
#15849=CARTESIAN_POINT('Origin',(0.685838782044607,-0.05953,-0.860014630714833));
#15850=CARTESIAN_POINT('Origin',(0.,-0.208355,0.));
#15851=CARTESIAN_POINT('',(-1.076188,-0.35718,1.31795018948079E-16));
#15852=CARTESIAN_POINT('Origin',(0.,-0.35718,0.));
#15853=CARTESIAN_POINT('',(-1.076188,-0.208355,1.31795018948079E-16));
#15854=CARTESIAN_POINT('',(1.03449977959455,-0.05953,0.296632461748266));
#15855=CARTESIAN_POINT('Origin',(0.,-0.05953,0.));
#15856=CARTESIAN_POINT('',(1.03449977959455,-0.05953,-0.296632461748266));
#15857=CARTESIAN_POINT('Ctrl Pts',(1.03449977959455,-0.05953,0.296632461748267));
#15858=CARTESIAN_POINT('Ctrl Pts',(1.03628691421076,-0.0925528133349865,
0.290399865505497));
#15859=CARTESIAN_POINT('Ctrl Pts',(1.03958665287714,-0.124911173756694,
0.278797079997872));
#15860=CARTESIAN_POINT('Ctrl Pts',(1.0470264474309,-0.177924977804098,0.249198913998601));
#15861=CARTESIAN_POINT('Ctrl Pts',(1.05084995891418,-0.199697230012983,
0.232935932341942));
#15862=CARTESIAN_POINT('Ctrl Pts',(1.05844771715377,-0.237895043532788,
0.195533155353269));
#15863=CARTESIAN_POINT('Ctrl Pts',(1.06220882929878,-0.254319232363049,
0.17438929156337));
#15864=CARTESIAN_POINT('Ctrl Pts',(1.06849922508772,-0.28018331644634,0.130252399648131));
#15865=CARTESIAN_POINT('Ctrl Pts',(1.07137013248666,-0.29104845371857,0.105070977154072));
#15866=CARTESIAN_POINT('Ctrl Pts',(1.07522652957392,-0.30527573347708,0.0525526752791107));
#15867=CARTESIAN_POINT('Ctrl Pts',(1.076188,-0.308638795020976,0.025214283908933));
#15868=CARTESIAN_POINT('Ctrl Pts',(1.076188,-0.308638795020976,-0.025214283908933));
#15869=CARTESIAN_POINT('Ctrl Pts',(1.07522652957392,-0.30527573347708,-0.0525526752791107));
#15870=CARTESIAN_POINT('Ctrl Pts',(1.07137013248666,-0.29104845371857,-0.105070977154072));
#15871=CARTESIAN_POINT('Ctrl Pts',(1.06849922508772,-0.28018331644634,-0.130252399648131));
#15872=CARTESIAN_POINT('Ctrl Pts',(1.06220882929878,-0.254319232363049,
-0.17438929156337));
#15873=CARTESIAN_POINT('Ctrl Pts',(1.05844771715377,-0.237895043532788,
-0.195533155353269));
#15874=CARTESIAN_POINT('Ctrl Pts',(1.05084995891418,-0.199697230012983,
-0.232935932341942));
#15875=CARTESIAN_POINT('Ctrl Pts',(1.0470264474309,-0.177924977804098,-0.249198913998601));
#15876=CARTESIAN_POINT('Ctrl Pts',(1.03958665287714,-0.124911173756694,
-0.278797079997872));
#15877=CARTESIAN_POINT('Ctrl Pts',(1.03628691421076,-0.0925528133349865,
-0.290399865505497));
#15878=CARTESIAN_POINT('Ctrl Pts',(1.03449977959455,-0.05953,-0.296632461748267));
#15879=CARTESIAN_POINT('Origin',(0.,-0.05953,0.));
#15880=CARTESIAN_POINT('Origin',(0.,-0.05953,0.));
#15881=CARTESIAN_POINT('Origin',(1.1,-0.05953,0.));
#15882=CARTESIAN_POINT('Origin',(1.1,0.,0.));
#15883=CARTESIAN_POINT('Origin',(1.1,-0.05953,0.));
#15884=CARTESIAN_POINT('Origin',(0.,-0.35718,0.));
#15885=CARTESIAN_POINT('Origin',(0.,-0.05953,0.));
#15886=CARTESIAN_POINT('',(0.,0.,0.));
#15887=CARTESIAN_POINT('Origin',(1.119765,0.495,0.));
#15888=CARTESIAN_POINT('',(-1.119765,0.495,-1.37131662304724E-16));
#15889=CARTESIAN_POINT('Origin',(0.,0.495,0.));
#15890=CARTESIAN_POINT('',(-1.085235,0.495,-1.32902956907268E-16));
#15891=CARTESIAN_POINT('Origin',(0.,0.495,0.));
#15892=CARTESIAN_POINT('Origin',(0.,0.4575,0.));
#15893=CARTESIAN_POINT('',(-1.119765,0.42,-1.37131662304724E-16));
#15894=CARTESIAN_POINT('Origin',(0.,0.42,0.));
#15895=CARTESIAN_POINT('',(-1.119765,0.4575,-1.37131662304724E-16));
#15896=CARTESIAN_POINT('Origin',(1.085235,0.42,0.));
#15897=CARTESIAN_POINT('',(-1.085235,0.42,-1.32902956907268E-16));
#15898=CARTESIAN_POINT('Origin',(0.,0.42,0.));
#15899=CARTESIAN_POINT('Origin',(0.,0.4575,0.));
#15900=CARTESIAN_POINT('',(-1.085235,0.4575,-1.32902956907268E-16));
#15901=CARTESIAN_POINT('Origin',(1.119765,-0.42,0.));
#15902=CARTESIAN_POINT('',(-1.119765,-0.42,-1.37131662304724E-16));
#15903=CARTESIAN_POINT('Origin',(0.,-0.42,0.));
#15904=CARTESIAN_POINT('',(-1.085235,-0.42,-1.32902956907268E-16));
#15905=CARTESIAN_POINT('Origin',(0.,-0.42,0.));
#15906=CARTESIAN_POINT('Origin',(0.,-0.4575,0.));
#15907=CARTESIAN_POINT('',(-1.119765,-0.495,-1.37131662304724E-16));
#15908=CARTESIAN_POINT('Origin',(0.,-0.495,0.));
#15909=CARTESIAN_POINT('',(-1.119765,-0.4575,-1.37131662304724E-16));
#15910=CARTESIAN_POINT('Origin',(1.085235,-0.495,0.));
#15911=CARTESIAN_POINT('',(-1.085235,-0.495,-1.32902956907268E-16));
#15912=CARTESIAN_POINT('Origin',(0.,-0.495,0.));
#15913=CARTESIAN_POINT('Origin',(0.,-0.4575,0.));
#15914=CARTESIAN_POINT('',(-1.085235,-0.4575,-1.32902956907268E-16));
#15915=CARTESIAN_POINT('',(0.,0.,0.));
#15916=CARTESIAN_POINT('',(0.,0.,0.));
#15917=CARTESIAN_POINT('',(0.,0.,0.));
#15918=CARTESIAN_POINT('',(0.,0.,0.));
#15919=CARTESIAN_POINT('',(0.,0.,0.));
#15920=CARTESIAN_POINT('',(0.,0.,0.));
#15921=CARTESIAN_POINT('Origin',(0.0866025403784439,-0.4,-0.15));
#15922=CARTESIAN_POINT('',(0.173205080756888,-0.4,0.));
#15923=CARTESIAN_POINT('',(0.0866025403784439,-0.4,-0.15));
#15924=CARTESIAN_POINT('',(0.173205080756888,-0.4,0.));
#15925=CARTESIAN_POINT('',(0.0866025403784439,-0.64,-0.15));
#15926=CARTESIAN_POINT('',(0.0866025403784439,-0.4,-0.15));
#15927=CARTESIAN_POINT('',(0.173205080756888,-0.64,0.));
#15928=CARTESIAN_POINT('',(0.173205080756888,-0.64,0.));
#15929=CARTESIAN_POINT('',(0.173205080756888,-0.4,0.));
#15930=CARTESIAN_POINT('Origin',(-0.0866025403784438,-0.4,-0.15));
#15931=CARTESIAN_POINT('',(-0.0866025403784438,-0.4,-0.15));
#15932=CARTESIAN_POINT('',(0.0866025403784439,-0.4,-0.15));
#15933=CARTESIAN_POINT('',(-0.0866025403784438,-0.64,-0.15));
#15934=CARTESIAN_POINT('',(-0.0866025403784438,-0.4,-0.15));
#15935=CARTESIAN_POINT('',(0.0866025403784439,-0.64,-0.15));
#15936=CARTESIAN_POINT('Origin',(-0.173205080756888,-0.4,-2.77555756156289E-17));
#15937=CARTESIAN_POINT('',(-0.173205080756888,-0.4,-2.12115047744981E-17));
#15938=CARTESIAN_POINT('',(-0.0866025403784438,-0.4,-0.15));
#15939=CARTESIAN_POINT('',(-0.173205080756888,-0.64,-2.77555756156289E-17));
#15940=CARTESIAN_POINT('',(-0.173205080756888,-0.4,-2.12115047744981E-17));
#15941=CARTESIAN_POINT('',(-0.0866025403784438,-0.64,-0.15));
#15942=CARTESIAN_POINT('Origin',(-0.0866025403784439,-0.4,0.15));
#15943=CARTESIAN_POINT('',(-0.0866025403784439,-0.4,0.15));
#15944=CARTESIAN_POINT('',(-0.173205080756888,-0.4,-2.12115047744981E-17));
#15945=CARTESIAN_POINT('',(-0.0866025403784439,-0.64,0.15));
#15946=CARTESIAN_POINT('',(-0.0866025403784439,-0.4,0.15));
#15947=CARTESIAN_POINT('',(-0.173205080756888,-0.64,-2.12115047744981E-17));
#15948=CARTESIAN_POINT('Origin',(0.0866025403784439,-0.4,0.15));
#15949=CARTESIAN_POINT('',(0.0866025403784439,-0.4,0.15));
#15950=CARTESIAN_POINT('',(-0.0866025403784439,-0.4,0.15));
#15951=CARTESIAN_POINT('',(0.0866025403784439,-0.64,0.15));
#15952=CARTESIAN_POINT('',(0.0866025403784439,-0.4,0.15));
#15953=CARTESIAN_POINT('',(-0.0866025403784439,-0.64,0.15));
#15954=CARTESIAN_POINT('Origin',(0.173205080756888,-0.4,0.));
#15955=CARTESIAN_POINT('',(0.0866025403784439,-0.4,0.15));
#15956=CARTESIAN_POINT('',(0.0866025403784439,-0.64,0.15));
#15957=CARTESIAN_POINT('Origin',(0.,-0.4,-2.77555756156289E-17));
#15958=CARTESIAN_POINT('Origin',(0.,-0.64,-2.77555756156289E-17));
#15959=CARTESIAN_POINT('Origin',(0.,-1.,0.));
#15960=CARTESIAN_POINT('',(-0.1954,-1.,2.39295984553393E-17));
#15961=CARTESIAN_POINT('Origin',(0.,-1.,0.));
#15962=CARTESIAN_POINT('Origin',(0.3,0.4,0.));
#15963=CARTESIAN_POINT('',(-0.3,0.4,-3.67394039744206E-17));
#15964=CARTESIAN_POINT('Origin',(0.,0.4,0.));
#15965=CARTESIAN_POINT('Origin',(0.,0.375,0.));
#15966=CARTESIAN_POINT('',(-0.35,0.35,-4.28626379701573E-17));
#15967=CARTESIAN_POINT('Origin',(0.,0.35,0.));
#15968=CARTESIAN_POINT('',(-0.325,0.375,-3.9801020972289E-17));
#15969=CARTESIAN_POINT('Origin',(0.,0.19,0.));
#15970=CARTESIAN_POINT('',(-0.35,0.03,-4.28626379701574E-17));
#15971=CARTESIAN_POINT('Origin',(0.,0.03,0.));
#15972=CARTESIAN_POINT('',(-0.35,0.19,-4.28626379701574E-17));
#15973=CARTESIAN_POINT('Origin',(0.,0.0149999999999999,0.));
#15974=CARTESIAN_POINT('',(-0.32,-3.29597460435593E-17,-3.91886975727153E-17));
#15975=CARTESIAN_POINT('Origin',(0.,0.,0.));
#15976=CARTESIAN_POINT('',(-0.335,0.0149999999999999,-4.10256677714363E-17));
#15977=CARTESIAN_POINT('Origin',(0.22,0.,0.));
#15978=CARTESIAN_POINT('',(-0.22,-6.93889390390723E-18,-2.69422295812418E-17));
#15979=CARTESIAN_POINT('Origin',(0.,0.,0.));
#15980=CARTESIAN_POINT('Origin',(0.,-0.02,0.));
#15981=CARTESIAN_POINT('',(-0.1954,-0.0492,2.39295984553393E-17));
#15982=CARTESIAN_POINT('Origin',(0.,-0.0492,0.));
#15983=CARTESIAN_POINT('',(-0.21,-0.02,-2.57175827820944E-17));
#15984=CARTESIAN_POINT('Origin',(0.,-0.8,0.));
#15985=CARTESIAN_POINT('',(-0.1954,-0.8,-2.39295984553393E-17));
#15986=CARTESIAN_POINT('',(0.,0.,0.));
#15987=CARTESIAN_POINT('Origin',(0.45,0.6,0.));
#15988=CARTESIAN_POINT('',(-0.45,0.6,-5.51091059616309E-17));
#15989=CARTESIAN_POINT('Origin',(0.,0.6,0.));
#15990=CARTESIAN_POINT('Origin',(0.,0.575,0.));
#15991=CARTESIAN_POINT('',(-0.5,0.55,-6.12323399573677E-17));
#15992=CARTESIAN_POINT('Origin',(0.,0.55,0.));
#15993=CARTESIAN_POINT('',(-0.475,0.575,-5.81707229594993E-17));
#15994=CARTESIAN_POINT('Origin',(0.,0.29,0.));
#15995=CARTESIAN_POINT('',(-0.5,0.0299999999999998,-6.12323399573677E-17));
#15996=CARTESIAN_POINT('Origin',(0.,0.0299999999999998,0.));
#15997=CARTESIAN_POINT('',(-0.5,0.29,-6.12323399573677E-17));
#15998=CARTESIAN_POINT('Origin',(0.,0.0150000000000001,0.));
#15999=CARTESIAN_POINT('',(-0.47,7.11236625150491E-17,-5.75583995599256E-17));
#16000=CARTESIAN_POINT('Origin',(0.,0.,0.));
#16001=CARTESIAN_POINT('',(-0.485,0.0150000000000001,-5.93953697586466E-17));
#16002=CARTESIAN_POINT('Origin',(0.32,0.,0.));
#16003=CARTESIAN_POINT('',(-0.32,-6.93889390390723E-18,-3.91886975727153E-17));
#16004=CARTESIAN_POINT('Origin',(0.,0.,0.));
#16005=CARTESIAN_POINT('Origin',(0.,-0.02,0.));
#16006=CARTESIAN_POINT('',(-0.2942,-0.0515999999999999,3.60291088309151E-17));
#16007=CARTESIAN_POINT('Origin',(0.,-0.0515999999999999,0.));
#16008=CARTESIAN_POINT('',(-0.31,-0.02,-3.7964050773568E-17));
#16009=CARTESIAN_POINT('Origin',(0.,-1.24,0.));
#16010=CARTESIAN_POINT('',(-0.2942,-2.4458,3.60291088309151E-17));
#16011=CARTESIAN_POINT('Origin',(0.,-2.4458,0.));
#16012=CARTESIAN_POINT('',(-0.2942,-1.24,-3.60291088309151E-17));
#16013=CARTESIAN_POINT('Origin',(0.,-2.47,0.));
#16014=CARTESIAN_POINT('',(-0.24,-2.5,-2.93915231795365E-17));
#16015=CARTESIAN_POINT('Origin',(0.,-2.5,0.));
#16016=CARTESIAN_POINT('',(-0.27,-2.47,-3.30654635769785E-17));
#16017=CARTESIAN_POINT('Origin',(0.,-2.5,0.));
#16018=CARTESIAN_POINT('Origin',(0.144337567297406,-0.6,-0.25));
#16019=CARTESIAN_POINT('',(0.288675134594813,-0.6,0.));
#16020=CARTESIAN_POINT('',(0.144337567297406,-0.6,-0.25));
#16021=CARTESIAN_POINT('',(0.288675134594813,-0.6,0.));
#16022=CARTESIAN_POINT('',(0.144337567297406,-0.96,-0.25));
#16023=CARTESIAN_POINT('',(0.144337567297406,-0.6,-0.25));
#16024=CARTESIAN_POINT('',(0.288675134594813,-0.96,0.));
#16025=CARTESIAN_POINT('',(0.288675134594813,-0.96,0.));
#16026=CARTESIAN_POINT('',(0.288675134594813,-0.6,0.));
#16027=CARTESIAN_POINT('Origin',(-0.144337567297406,-0.6,-0.25));
#16028=CARTESIAN_POINT('',(-0.144337567297406,-0.6,-0.25));
#16029=CARTESIAN_POINT('',(0.144337567297406,-0.6,-0.25));
#16030=CARTESIAN_POINT('',(-0.144337567297406,-0.96,-0.25));
#16031=CARTESIAN_POINT('',(-0.144337567297406,-0.6,-0.25));
#16032=CARTESIAN_POINT('',(0.144337567297406,-0.96,-0.25));
#16033=CARTESIAN_POINT('Origin',(-0.288675134594813,-0.6,-8.32667268468867E-17));
#16034=CARTESIAN_POINT('',(-0.288675134594813,-0.6,-3.53525079574969E-17));
#16035=CARTESIAN_POINT('',(-0.144337567297406,-0.6,-0.25));
#16036=CARTESIAN_POINT('',(-0.288675134594813,-0.96,-5.55111512312578E-17));
#16037=CARTESIAN_POINT('',(-0.288675134594813,-0.6,-3.53525079574969E-17));
#16038=CARTESIAN_POINT('',(-0.144337567297406,-0.96,-0.25));
#16039=CARTESIAN_POINT('Origin',(-0.144337567297407,-0.6,0.25));
#16040=CARTESIAN_POINT('',(-0.144337567297407,-0.6,0.25));
#16041=CARTESIAN_POINT('',(-0.288675134594813,-0.6,-3.53525079574969E-17));
#16042=CARTESIAN_POINT('',(-0.144337567297407,-0.96,0.25));
#16043=CARTESIAN_POINT('',(-0.144337567297407,-0.6,0.25));
#16044=CARTESIAN_POINT('',(-0.288675134594813,-0.96,-3.53525079574969E-17));
#16045=CARTESIAN_POINT('Origin',(0.144337567297406,-0.6,0.25));
#16046=CARTESIAN_POINT('',(0.144337567297406,-0.6,0.25));
#16047=CARTESIAN_POINT('',(-0.144337567297407,-0.6,0.25));
#16048=CARTESIAN_POINT('',(0.144337567297406,-0.96,0.25));
#16049=CARTESIAN_POINT('',(0.144337567297406,-0.6,0.25));
#16050=CARTESIAN_POINT('',(-0.144337567297407,-0.96,0.25));
#16051=CARTESIAN_POINT('Origin',(0.288675134594813,-0.6,0.));
#16052=CARTESIAN_POINT('',(0.144337567297406,-0.6,0.25));
#16053=CARTESIAN_POINT('',(0.144337567297406,-0.96,0.25));
#16054=CARTESIAN_POINT('Origin',(0.,-0.6,0.));
#16055=CARTESIAN_POINT('Origin',(0.,-0.96,0.));
#16056=CARTESIAN_POINT('',(0.,0.,0.));
#16057=CARTESIAN_POINT('Origin',(0.,0.0584134911936118,0.));
#16058=CARTESIAN_POINT('',(-0.288675134594813,0.0590919554682611,0.5));
#16059=CARTESIAN_POINT('',(0.288675134594813,0.0590919554682611,0.5));
#16060=CARTESIAN_POINT('Ctrl Pts',(-0.288675134594813,0.0590919554682611,
0.5));
#16061=CARTESIAN_POINT('Ctrl Pts',(2.1664336991023E-12,-0.0242413778636964,
0.5));
#16062=CARTESIAN_POINT('Ctrl Pts',(0.288675134594813,0.0590919554682611,
0.5));
#16063=CARTESIAN_POINT('',(-0.577350269189626,0.0590919554682611,-7.07050159149938E-17));
#16064=CARTESIAN_POINT('Ctrl Pts',(-0.577350269189626,0.0590919554682611,
-7.07050159149938E-17));
#16065=CARTESIAN_POINT('Ctrl Pts',(-0.433012701891136,-0.0242413778636963,
0.250000000001876));
#16066=CARTESIAN_POINT('Ctrl Pts',(-0.288675134594813,0.0590919554682611,
0.5));
#16067=CARTESIAN_POINT('',(-0.475,-4.16333634234434E-17,-5.81707229594993E-17));
#16068=CARTESIAN_POINT('',(-0.576175134594813,0.0584134911936118,-7.05611034329833E-17));
#16069=CARTESIAN_POINT('Origin',(0.,0.,0.));
#16070=CARTESIAN_POINT('',(-0.288675134594813,0.0590919554682611,-0.5));
#16071=CARTESIAN_POINT('Ctrl Pts',(-0.288675134594813,0.0590919554682611,
-0.5));
#16072=CARTESIAN_POINT('Ctrl Pts',(-0.433012701893303,-0.0242413778636963,
-0.249999999998124));
#16073=CARTESIAN_POINT('Ctrl Pts',(-0.577350269189626,0.0590919554682611,
-7.07050159149938E-17));
#16074=CARTESIAN_POINT('',(0.288675134594813,0.0590919554682611,-0.5));
#16075=CARTESIAN_POINT('Ctrl Pts',(0.288675134594813,0.0590919554682611,
-0.5));
#16076=CARTESIAN_POINT('Ctrl Pts',(-2.16648921025353E-12,-0.0242413778636962,
-0.5));
#16077=CARTESIAN_POINT('Ctrl Pts',(-0.288675134594813,0.0590919554682611,
-0.5));
#16078=CARTESIAN_POINT('',(0.577350269189626,0.0590919554682611,0.));
#16079=CARTESIAN_POINT('Ctrl Pts',(0.577350269189626,0.0590919554682611,
0.));
#16080=CARTESIAN_POINT('Ctrl Pts',(0.433012701891136,-0.0242413778636963,
-0.250000000001876));
#16081=CARTESIAN_POINT('Ctrl Pts',(0.288675134594813,0.0590919554682611,
-0.5));
#16082=CARTESIAN_POINT('Ctrl Pts',(0.288675134594813,0.0590919554682611,
0.5));
#16083=CARTESIAN_POINT('Ctrl Pts',(0.433012701893303,-0.0242413778636962,
0.249999999998124));
#16084=CARTESIAN_POINT('Ctrl Pts',(0.577350269189626,0.0590919554682611,
0.));
#16085=CARTESIAN_POINT('Origin',(0.,0.461586508806388,0.));
#16086=CARTESIAN_POINT('',(-0.475,0.52,-5.81707229594993E-17));
#16087=CARTESIAN_POINT('Origin',(0.,0.52,0.));
#16088=CARTESIAN_POINT('',(-0.577350269189626,0.460908044531739,-7.07050159149938E-17));
#16089=CARTESIAN_POINT('',(-0.576175134594813,0.461586508806388,-7.05611034329833E-17));
#16090=CARTESIAN_POINT('',(-0.288675134594813,0.460908044531739,0.5));
#16091=CARTESIAN_POINT('Ctrl Pts',(-0.288675134594813,0.460908044531739,
0.5));
#16092=CARTESIAN_POINT('Ctrl Pts',(-0.433012701893303,0.544241377863696,
0.249999999998124));
#16093=CARTESIAN_POINT('Ctrl Pts',(-0.577350269189626,0.460908044531739,
-7.07050159149938E-17));
#16094=CARTESIAN_POINT('',(0.288675134594813,0.460908044531739,0.5));
#16095=CARTESIAN_POINT('Ctrl Pts',(0.288675134594813,0.460908044531739,
0.5));
#16096=CARTESIAN_POINT('Ctrl Pts',(-2.16676676600969E-12,0.544241377863697,
0.5));
#16097=CARTESIAN_POINT('Ctrl Pts',(-0.288675134594813,0.460908044531739,
0.5));
#16098=CARTESIAN_POINT('',(0.577350269189626,0.460908044531739,0.));
#16099=CARTESIAN_POINT('Ctrl Pts',(0.577350269189626,0.460908044531739,
0.));
#16100=CARTESIAN_POINT('Ctrl Pts',(0.433012701891136,0.544241377863696,
0.250000000001876));
#16101=CARTESIAN_POINT('Ctrl Pts',(0.288675134594813,0.460908044531739,
0.5));
#16102=CARTESIAN_POINT('',(0.288675134594813,0.460908044531739,-0.5));
#16103=CARTESIAN_POINT('Ctrl Pts',(0.288675134594813,0.460908044531739,
-0.5));
#16104=CARTESIAN_POINT('Ctrl Pts',(0.433012701893302,0.544241377863696,
-0.249999999998124));
#16105=CARTESIAN_POINT('Ctrl Pts',(0.577350269189626,0.460908044531739,
0.));
#16106=CARTESIAN_POINT('',(-0.288675134594813,0.460908044531739,-0.5));
#16107=CARTESIAN_POINT('Ctrl Pts',(-0.288675134594813,0.460908044531739,
-0.5));
#16108=CARTESIAN_POINT('Ctrl Pts',(2.16660023255599E-12,0.544241377863697,
-0.5));
#16109=CARTESIAN_POINT('Ctrl Pts',(0.288675134594813,0.460908044531739,
-0.5));
#16110=CARTESIAN_POINT('Ctrl Pts',(-0.577350269189626,0.460908044531739,
-7.07050159149938E-17));
#16111=CARTESIAN_POINT('Ctrl Pts',(-0.433012701891136,0.544241377863696,
-0.250000000001876));
#16112=CARTESIAN_POINT('Ctrl Pts',(-0.288675134594813,0.460908044531739,
-0.5));
#16113=CARTESIAN_POINT('Origin',(0.288675134594813,0.,-0.5));
#16114=CARTESIAN_POINT('',(-0.288675134594813,0.,-0.5));
#16115=CARTESIAN_POINT('',(0.288675134594813,0.,-0.5));
#16116=CARTESIAN_POINT('Origin',(-0.288675134594813,0.,-0.5));
#16117=CARTESIAN_POINT('',(-0.577350269189626,0.,-7.07050159149938E-17));
#16118=CARTESIAN_POINT('Origin',(-0.577350269189626,0.,-7.07050159149938E-17));
#16119=CARTESIAN_POINT('',(-0.288675134594813,0.,0.5));
#16120=CARTESIAN_POINT('Origin',(0.,0.,0.));
#16121=CARTESIAN_POINT('',(-0.25175,0.52,3.08304831685346E-17));
#16122=CARTESIAN_POINT('Origin',(0.,0.52,0.));
#16123=CARTESIAN_POINT('',(-0.25175,0.,3.08304831685346E-17));
#16124=CARTESIAN_POINT('',(-0.25175,0.,3.08304831685346E-17));
#16125=CARTESIAN_POINT('Origin',(0.,0.,0.));
#16126=CARTESIAN_POINT('Origin',(-0.288675134594813,0.,0.5));
#16127=CARTESIAN_POINT('',(0.288675134594813,0.,0.5));
#16128=CARTESIAN_POINT('Origin',(0.577350269189626,0.,0.));
#16129=CARTESIAN_POINT('',(0.577350269189626,0.,0.));
#16130=CARTESIAN_POINT('Origin',(0.288675134594813,0.,0.5));
#16131=CARTESIAN_POINT('Origin',(0.,0.52,0.));
#16132=CARTESIAN_POINT('Origin',(0.,0.,0.));
#16133=CARTESIAN_POINT('',(0.,0.,0.));
#16134=CARTESIAN_POINT('',(0.,0.,0.));
#16135=CARTESIAN_POINT('Origin',(0.,-1.4,7.));
#16136=CARTESIAN_POINT('',(-0.165,-1.4,7.));
#16137=CARTESIAN_POINT('Origin',(0.,-1.4,7.));
#16138=CARTESIAN_POINT('',(-0.165,0.,7.));
#16139=CARTESIAN_POINT('',(-0.165,-1.4,7.));
#16140=CARTESIAN_POINT('Origin',(0.,0.,7.));
#16141=CARTESIAN_POINT('Origin',(0.,-1.4,7.));
#16142=CARTESIAN_POINT('Origin',(-0.2,-1.8,6.3));
#16143=CARTESIAN_POINT('',(-0.2,-0.4,6.43431457505076));
#16144=CARTESIAN_POINT('',(-0.2,-1.8,6.43431457505076));
#16145=CARTESIAN_POINT('',(-0.2,-9.,6.43431457505076));
#16146=CARTESIAN_POINT('',(-0.2,-0.4,6.65));
#16147=CARTESIAN_POINT('',(-0.2,-0.4,6.65));
#16148=CARTESIAN_POINT('',(-0.2,-1.8,6.65));
#16149=CARTESIAN_POINT('',(-0.2,-1.8,6.65));
#16150=CARTESIAN_POINT('',(-0.2,-1.8,6.65));
#16151=CARTESIAN_POINT('Origin',(0.,-1.8,6.475));
#16152=CARTESIAN_POINT('',(0.2,-1.8,6.43431457505076));
#16153=CARTESIAN_POINT('Origin',(0.,-1.8,7.));
#16154=CARTESIAN_POINT('',(0.2,-1.8,6.65));
#16155=CARTESIAN_POINT('',(0.2,-1.8,6.65));
#16156=CARTESIAN_POINT('',(0.2,-1.8,6.3));
#16157=CARTESIAN_POINT('Origin',(0.2,-1.8,6.65));
#16158=CARTESIAN_POINT('',(0.2,-0.4,6.43431457505076));
#16159=CARTESIAN_POINT('',(0.2,-9.,6.43431457505076));
#16160=CARTESIAN_POINT('',(0.2,-0.4,6.65));
#16161=CARTESIAN_POINT('',(0.2,-1.8,6.65));
#16162=CARTESIAN_POINT('',(0.2,-0.4,6.3));
#16163=CARTESIAN_POINT('Origin',(-0.2,-1.8,6.65));
#16164=CARTESIAN_POINT('',(0.2,-0.4,6.65));
#16165=CARTESIAN_POINT('Origin',(0.,-0.4,6.475));
#16166=CARTESIAN_POINT('Origin',(0.,-0.4,7.));
#16167=CARTESIAN_POINT('Origin',(0.,-2.,7.));
#16168=CARTESIAN_POINT('',(-0.8,-2.,7.));
#16169=CARTESIAN_POINT('Origin',(0.,-2.,7.));
#16170=CARTESIAN_POINT('',(-0.6,-2.,7.));
#16171=CARTESIAN_POINT('Origin',(0.,-2.,7.));
#16172=CARTESIAN_POINT('Origin',(0.,-3.5,7.));
#16173=CARTESIAN_POINT('',(-0.8,-3.5,7.));
#16174=CARTESIAN_POINT('Origin',(0.,-3.5,7.));
#16175=CARTESIAN_POINT('',(-0.6,-3.5,7.));
#16176=CARTESIAN_POINT('Origin',(0.,-3.5,7.));
#16177=CARTESIAN_POINT('Origin',(0.,-3.5,7.));
#16178=CARTESIAN_POINT('',(-0.8,-3.5,7.));
#16179=CARTESIAN_POINT('Origin',(0.,-9.,7.));
#16180=CARTESIAN_POINT('',(-0.6,-9.,7.));
#16181=CARTESIAN_POINT('',(-0.6,-9.,7.));
#16182=CARTESIAN_POINT('Origin',(0.,-9.,7.));
#16183=CARTESIAN_POINT('Origin',(0.,-9.,7.));
#16184=CARTESIAN_POINT('',(-0.6,0.,7.));
#16185=CARTESIAN_POINT('Origin',(0.,0.,7.));
#16186=CARTESIAN_POINT('',(-0.6,-9.,7.));
#16187=CARTESIAN_POINT('Origin',(0.,0.,7.));
#16188=CARTESIAN_POINT('Origin',(0.,-9.,7.));
#16189=CARTESIAN_POINT('',(0.,0.,0.));
#16190=CARTESIAN_POINT('Origin',(0.,-6.5,7.));
#16191=CARTESIAN_POINT('',(-0.605,-4.5,7.));
#16192=CARTESIAN_POINT('Origin',(0.,-4.5,7.));
#16193=CARTESIAN_POINT('',(-0.605,-6.5,7.));
#16194=CARTESIAN_POINT('',(-0.605,-6.5,7.));
#16195=CARTESIAN_POINT('Origin',(0.,-6.5,7.));
#16196=CARTESIAN_POINT('Origin',(0.,-6.5,7.));
#16197=CARTESIAN_POINT('',(-0.8,-4.5,7.));
#16198=CARTESIAN_POINT('Origin',(0.,-4.5,7.));
#16199=CARTESIAN_POINT('',(-0.8,-6.5,7.));
#16200=CARTESIAN_POINT('',(-0.8,-6.5,7.));
#16201=CARTESIAN_POINT('Origin',(0.,-6.5,7.));
#16202=CARTESIAN_POINT('Origin',(0.,-4.5,7.));
#16203=CARTESIAN_POINT('Origin',(0.,-6.5,7.));
#16204=CARTESIAN_POINT('',(0.,0.,0.));
#16205=CARTESIAN_POINT('Origin',(0.,-7.9,7.59));
#16206=CARTESIAN_POINT('',(0.133884278389956,-8.06178689687364,7.59));
#16207=CARTESIAN_POINT('',(0.133884278389956,-7.73821310312636,7.59));
#16208=CARTESIAN_POINT('',(0.133884278389956,-8.3,7.59));
#16209=CARTESIAN_POINT('Origin',(0.,-7.9,7.59));
#16210=CARTESIAN_POINT('Origin',(0.,-7.9,7.59));
#16211=CARTESIAN_POINT('',(-0.133884278389956,-8.06178689687364,7.59));
#16212=CARTESIAN_POINT('Ctrl Pts',(-0.133884278389956,-8.06178689687364,
7.59));
#16213=CARTESIAN_POINT('Ctrl Pts',(-0.118254395260802,-8.07472116821763,
7.59354677224418));
#16214=CARTESIAN_POINT('Ctrl Pts',(-0.100109787682299,-8.08579931658744,
7.59698224789957));
#16215=CARTESIAN_POINT('Ctrl Pts',(-0.054829872132519,-8.10463856105443,
7.6030741628997));
#16216=CARTESIAN_POINT('Ctrl Pts',(-0.0266020595922904,-8.11,7.605));
#16217=CARTESIAN_POINT('Ctrl Pts',(0.0266020595922903,-8.11,7.605));
#16218=CARTESIAN_POINT('Ctrl Pts',(0.0548298721325189,-8.10463856105443,
7.6030741628997));
#16219=CARTESIAN_POINT('Ctrl Pts',(0.100109787682299,-8.08579931658744,
7.59698224789957));
#16220=CARTESIAN_POINT('Ctrl Pts',(0.118254395260802,-8.07472116821763,
7.59354677224418));
#16221=CARTESIAN_POINT('Ctrl Pts',(0.133884278389957,-8.06178689687364,
7.59));
#16222=CARTESIAN_POINT('',(-0.21,-7.9,7.59));
#16223=CARTESIAN_POINT('Origin',(0.,-7.9,7.59));
#16224=CARTESIAN_POINT('',(-0.21,-7.9,8.07976849370594));
#16225=CARTESIAN_POINT('',(-0.21,-7.9,7.59));
#16226=CARTESIAN_POINT('',(0.21,-7.9,8.07976849370594));
#16227=CARTESIAN_POINT('Ctrl Pts',(0.21,-7.9,8.07976849370594));
#16228=CARTESIAN_POINT('Ctrl Pts',(0.21,-7.92643858813051,8.07976849370594));
#16229=CARTESIAN_POINT('Ctrl Pts',(0.204702922670977,-7.95459378125493,
8.08084015664674));
#16230=CARTESIAN_POINT('Ctrl Pts',(0.183251796806355,-8.00631344554134,
8.08468313707126));
#16231=CARTESIAN_POINT('Ctrl Pts',(0.167101177357214,-8.02988367074114,
8.08739593054622));
#16232=CARTESIAN_POINT('Ctrl Pts',(0.129884533480965,-8.06710031461738,
8.09246633289124));
#16233=CARTESIAN_POINT('Ctrl Pts',(0.106313940757289,-8.08325161016341,
8.09515738895358));
#16234=CARTESIAN_POINT('Ctrl Pts',(0.0545930033295209,-8.10470322656974,
8.09895039220591));
#16235=CARTESIAN_POINT('Ctrl Pts',(0.0264373623835353,-8.11,8.1));
#16236=CARTESIAN_POINT('Ctrl Pts',(-0.0264373623835353,-8.11,8.1));
#16237=CARTESIAN_POINT('Ctrl Pts',(-0.0545930033295208,-8.10470322656974,
8.09895039220591));
#16238=CARTESIAN_POINT('Ctrl Pts',(-0.106313940757289,-8.08325161016341,
8.09515738895358));
#16239=CARTESIAN_POINT('Ctrl Pts',(-0.129884533480965,-8.06710031461738,
8.09246633289124));
#16240=CARTESIAN_POINT('Ctrl Pts',(-0.167101177357214,-8.02988367074114,
8.08739593054622));
#16241=CARTESIAN_POINT('Ctrl Pts',(-0.183251796806355,-8.00631344554134,
8.08468313707126));
#16242=CARTESIAN_POINT('Ctrl Pts',(-0.204702922670977,-7.95459378125493,
8.08084015664674));
#16243=CARTESIAN_POINT('Ctrl Pts',(-0.21,-7.92643858813051,8.07976849370594));
#16244=CARTESIAN_POINT('Ctrl Pts',(-0.21,-7.9,8.07976849370594));
#16245=CARTESIAN_POINT('Ctrl Pts',(-0.21,-7.9,8.07976849370594));
#16246=CARTESIAN_POINT('Ctrl Pts',(-0.21,-7.87356141186949,8.07976849370594));
#16247=CARTESIAN_POINT('Ctrl Pts',(-0.204702922670977,-7.84540621874507,
8.08084015664674));
#16248=CARTESIAN_POINT('Ctrl Pts',(-0.183251796806355,-7.79368655445866,
8.08468313707126));
#16249=CARTESIAN_POINT('Ctrl Pts',(-0.167101177357215,-7.77011632925886,
8.08739593054622));
#16250=CARTESIAN_POINT('Ctrl Pts',(-0.129884533480965,-7.73289968538262,
8.09246633289124));
#16251=CARTESIAN_POINT('Ctrl Pts',(-0.106313940757289,-7.71674838983659,
8.09515738895358));
#16252=CARTESIAN_POINT('Ctrl Pts',(-0.054593003329521,-7.69529677343026,
8.09895039220591));
#16253=CARTESIAN_POINT('Ctrl Pts',(-0.0264373623835353,-7.69,8.1));
#16254=CARTESIAN_POINT('Ctrl Pts',(0.0264373623835353,-7.69,8.1));
#16255=CARTESIAN_POINT('Ctrl Pts',(0.0545930033295201,-7.69529677343026,
8.09895039220591));
#16256=CARTESIAN_POINT('Ctrl Pts',(0.106313940757288,-7.71674838983659,
8.09515738895358));
#16257=CARTESIAN_POINT('Ctrl Pts',(0.129884533480965,-7.73289968538262,
8.09246633289124));
#16258=CARTESIAN_POINT('Ctrl Pts',(0.167101177357214,-7.77011632925886,
8.08739593054622));
#16259=CARTESIAN_POINT('Ctrl Pts',(0.183251796806355,-7.79368655445866,
8.08468313707126));
#16260=CARTESIAN_POINT('Ctrl Pts',(0.204702922670977,-7.84540621874507,
8.08084015664674));
#16261=CARTESIAN_POINT('Ctrl Pts',(0.21,-7.87356141186949,8.07976849370594));
#16262=CARTESIAN_POINT('Ctrl Pts',(0.21,-7.9,8.07976849370594));
#16263=CARTESIAN_POINT('',(-0.133884278389956,-7.73821310312636,7.59));
#16264=CARTESIAN_POINT('Origin',(0.,-7.9,7.59));
#16265=CARTESIAN_POINT('Ctrl Pts',(0.133884278389956,-7.73821310312636,
7.59));
#16266=CARTESIAN_POINT('Ctrl Pts',(0.118254395260802,-7.72527883178237,
7.59354677224418));
#16267=CARTESIAN_POINT('Ctrl Pts',(0.100109787682299,-7.71420068341256,
7.59698224789957));
#16268=CARTESIAN_POINT('Ctrl Pts',(0.0548298721325194,-7.69536143894557,
7.6030741628997));
#16269=CARTESIAN_POINT('Ctrl Pts',(0.0266020595922903,-7.69,7.605));
#16270=CARTESIAN_POINT('Ctrl Pts',(-0.0266020595922902,-7.69,7.605));
#16271=CARTESIAN_POINT('Ctrl Pts',(-0.0548298721325196,-7.69536143894557,
7.6030741628997));
#16272=CARTESIAN_POINT('Ctrl Pts',(-0.100109787682299,-7.71420068341256,
7.59698224789957));
#16273=CARTESIAN_POINT('Ctrl Pts',(-0.118254395260801,-7.72527883178237,
7.59354677224418));
#16274=CARTESIAN_POINT('Ctrl Pts',(-0.133884278389955,-7.73821310312636,
7.59));
#16275=CARTESIAN_POINT('Origin',(0.,-7.9,7.59));
#16276=CARTESIAN_POINT('',(-0.133884278389956,-8.3,7.59));
#16277=CARTESIAN_POINT('Origin',(0.,-8.3,7.));
#16278=CARTESIAN_POINT('',(-0.605,-7.5,7.));
#16279=CARTESIAN_POINT('Origin',(0.,-7.5,7.));
#16280=CARTESIAN_POINT('',(-0.605,-8.3,7.));
#16281=CARTESIAN_POINT('',(-0.605,-8.3,7.));
#16282=CARTESIAN_POINT('Origin',(0.,-8.3,7.));
#16283=CARTESIAN_POINT('Origin',(0.,-8.3,7.));
#16284=CARTESIAN_POINT('',(-1.1,-7.5,7.));
#16285=CARTESIAN_POINT('Origin',(0.,-7.5,7.));
#16286=CARTESIAN_POINT('',(-1.1,-8.3,7.));
#16287=CARTESIAN_POINT('',(-1.1,-8.3,7.));
#16288=CARTESIAN_POINT('Origin',(0.,-8.3,7.));
#16289=CARTESIAN_POINT('Origin',(0.,-7.5,7.));
#16290=CARTESIAN_POINT('Origin',(0.,-8.3,7.));
#16291=CARTESIAN_POINT('',(0.,0.,0.));
#16292=CARTESIAN_POINT('Origin',(-0.2,-2.1,6.22));
#16293=CARTESIAN_POINT('',(-0.2,-2.,6.22));
#16294=CARTESIAN_POINT('',(-0.2,-2.,6.43431457505076));
#16295=CARTESIAN_POINT('',(-0.2,-2.,6.61));
#16296=CARTESIAN_POINT('',(-0.2,-0.1,6.22));
#16297=CARTESIAN_POINT('',(-0.2,-2.1,6.22));
#16298=CARTESIAN_POINT('',(-0.2,-0.1,6.43431457505076));
#16299=CARTESIAN_POINT('',(-0.2,-0.0999999999999999,6.61));
#16300=CARTESIAN_POINT('',(-0.2,-2.,6.43431457505076));
#16301=CARTESIAN_POINT('Origin',(0.2,-2.1,6.22));
#16302=CARTESIAN_POINT('',(0.2,-2.,6.22));
#16303=CARTESIAN_POINT('',(0.1,-2.,6.22));
#16304=CARTESIAN_POINT('',(0.2,-0.1,6.22));
#16305=CARTESIAN_POINT('',(0.2,-2.1,6.22));
#16306=CARTESIAN_POINT('',(0.1,-0.0999999999999999,6.22));
#16307=CARTESIAN_POINT('Origin',(0.2,-2.1,7.));
#16308=CARTESIAN_POINT('',(0.2,-2.,6.43431457505076));
#16309=CARTESIAN_POINT('',(0.2,-2.,7.));
#16310=CARTESIAN_POINT('',(0.2,-0.1,6.43431457505076));
#16311=CARTESIAN_POINT('',(0.2,-2.,6.43431457505076));
#16312=CARTESIAN_POINT('',(0.2,-0.0999999999999999,7.));
#16313=CARTESIAN_POINT('Origin',(0.,-0.0999999999999999,7.));
#16314=CARTESIAN_POINT('',(-3.,-0.1,7.));
#16315=CARTESIAN_POINT('Origin',(0.,-0.1,7.));
#16316=CARTESIAN_POINT('Origin',(0.,-0.0999999999999999,7.));
#16317=CARTESIAN_POINT('Origin',(0.,-2.,7.));
#16318=CARTESIAN_POINT('Origin',(0.,-2.,7.));
#16319=CARTESIAN_POINT('Origin',(0.,-0.8,7.));
#16320=CARTESIAN_POINT('',(-3.,-0.8,7.));
#16321=CARTESIAN_POINT('Origin',(0.,-0.8,7.));
#16322=CARTESIAN_POINT('',(-1.2,-0.8,7.));
#16323=CARTESIAN_POINT('Origin',(0.,-0.8,7.));
#16324=CARTESIAN_POINT('Origin',(0.,-0.8,7.));
#16325=CARTESIAN_POINT('',(-3.,-0.8,7.));
#16326=CARTESIAN_POINT('Origin',(0.,-2.,7.));
#16327=CARTESIAN_POINT('',(-1.2,-2.,7.));
#16328=CARTESIAN_POINT('',(-1.2,-2.,7.));
#16329=CARTESIAN_POINT('Origin',(0.,-2.,7.));
#16330=CARTESIAN_POINT('Origin',(0.,-2.,7.));
#16331=CARTESIAN_POINT('',(0.,0.,0.));
#16332=CARTESIAN_POINT('Origin',(0.,-0.1,7.));
#16333=CARTESIAN_POINT('',(-0.605,0.,7.));
#16334=CARTESIAN_POINT('Origin',(0.,0.,7.));
#16335=CARTESIAN_POINT('',(-0.605,-0.1,7.));
#16336=CARTESIAN_POINT('',(-0.605,-0.1,7.));
#16337=CARTESIAN_POINT('Origin',(0.,-0.1,7.));
#16338=CARTESIAN_POINT('Origin',(0.,-0.1,7.));
#16339=CARTESIAN_POINT('',(-3.,0.,7.));
#16340=CARTESIAN_POINT('Origin',(0.,0.,7.));
#16341=CARTESIAN_POINT('',(-3.,-0.1,7.));
#16342=CARTESIAN_POINT('',(-3.,-0.1,7.));
#16343=CARTESIAN_POINT('Origin',(0.,-0.1,7.));
#16344=CARTESIAN_POINT('Origin',(0.,0.,7.));
#16345=CARTESIAN_POINT('Origin',(0.,-0.1,7.));
#16346=CARTESIAN_POINT('',(0.,0.,0.));
#16347=CARTESIAN_POINT('Origin',(0.,0.,7.));
#16348=CARTESIAN_POINT('',(-0.225,0.2,7.));
#16349=CARTESIAN_POINT('Origin',(0.,0.2,7.));
#16350=CARTESIAN_POINT('',(-0.225,0.,7.));
#16351=CARTESIAN_POINT('',(-0.225,0.,7.));
#16352=CARTESIAN_POINT('Origin',(0.,0.,7.));
#16353=CARTESIAN_POINT('Origin',(0.,0.,7.));
#16354=CARTESIAN_POINT('',(-0.9,0.2,7.));
#16355=CARTESIAN_POINT('Origin',(0.,0.2,7.));
#16356=CARTESIAN_POINT('',(-0.9,0.,7.));
#16357=CARTESIAN_POINT('',(-0.9,0.,7.));
#16358=CARTESIAN_POINT('Origin',(0.,0.,7.));
#16359=CARTESIAN_POINT('Origin',(0.,0.2,7.));
#16360=CARTESIAN_POINT('Origin',(0.,0.,7.));
#16361=CARTESIAN_POINT('',(0.,0.,0.));
#16362=CARTESIAN_POINT('Origin',(0.3,0.4,0.));
#16363=CARTESIAN_POINT('',(-0.3,0.4,-3.67394039744206E-17));
#16364=CARTESIAN_POINT('Origin',(0.,0.4,0.));
#16365=CARTESIAN_POINT('Origin',(0.,0.375,0.));
#16366=CARTESIAN_POINT('',(-0.35,0.35,-4.28626379701573E-17));
#16367=CARTESIAN_POINT('Origin',(0.,0.35,0.));
#16368=CARTESIAN_POINT('',(-0.325,0.375,-3.9801020972289E-17));
#16369=CARTESIAN_POINT('Origin',(0.,0.19,0.));
#16370=CARTESIAN_POINT('',(-0.35,0.03,-4.28626379701574E-17));
#16371=CARTESIAN_POINT('Origin',(0.,0.03,0.));
#16372=CARTESIAN_POINT('',(-0.35,0.19,-4.28626379701574E-17));
#16373=CARTESIAN_POINT('Origin',(0.,0.0149999999999999,0.));
#16374=CARTESIAN_POINT('',(-0.32,-3.29597460435593E-17,-3.91886975727153E-17));
#16375=CARTESIAN_POINT('Origin',(0.,0.,0.));
#16376=CARTESIAN_POINT('',(-0.335,0.0149999999999999,-4.10256677714363E-17));
#16377=CARTESIAN_POINT('Origin',(0.22,0.,0.));
#16378=CARTESIAN_POINT('',(-0.22,-6.93889390390723E-18,-2.69422295812418E-17));
#16379=CARTESIAN_POINT('Origin',(0.,0.,0.));
#16380=CARTESIAN_POINT('Origin',(0.,-0.02,0.));
#16381=CARTESIAN_POINT('',(-0.1954,-0.0492,2.39295984553393E-17));
#16382=CARTESIAN_POINT('Origin',(0.,-0.0492,0.));
#16383=CARTESIAN_POINT('',(-0.21,-0.02,-2.57175827820944E-17));
#16384=CARTESIAN_POINT('Origin',(0.,-0.8,0.));
#16385=CARTESIAN_POINT('',(-0.1954,-1.5646,2.39295984553393E-17));
#16386=CARTESIAN_POINT('Origin',(0.,-1.5646,0.));
#16387=CARTESIAN_POINT('',(-0.1954,-0.8,-2.39295984553393E-17));
#16388=CARTESIAN_POINT('Origin',(0.,-1.58,0.));
#16389=CARTESIAN_POINT('',(-0.16,-1.6,-1.95943487863577E-17));
#16390=CARTESIAN_POINT('Origin',(0.,-1.6,0.));
#16391=CARTESIAN_POINT('',(-0.18,-1.58,-2.20436423846524E-17));
#16392=CARTESIAN_POINT('Origin',(0.,-1.6,0.));
#16393=CARTESIAN_POINT('Origin',(0.0866025403784439,-0.4,-0.15));
#16394=CARTESIAN_POINT('',(0.173205080756888,-0.4,0.));
#16395=CARTESIAN_POINT('',(0.0866025403784439,-0.4,-0.15));
#16396=CARTESIAN_POINT('',(0.173205080756888,-0.4,0.));
#16397=CARTESIAN_POINT('',(0.0866025403784439,-0.64,-0.15));
#16398=CARTESIAN_POINT('',(0.0866025403784439,-0.4,-0.15));
#16399=CARTESIAN_POINT('',(0.173205080756888,-0.64,0.));
#16400=CARTESIAN_POINT('',(0.173205080756888,-0.64,0.));
#16401=CARTESIAN_POINT('',(0.173205080756888,-0.4,0.));
#16402=CARTESIAN_POINT('Origin',(-0.0866025403784438,-0.4,-0.15));
#16403=CARTESIAN_POINT('',(-0.0866025403784438,-0.4,-0.15));
#16404=CARTESIAN_POINT('',(0.0866025403784439,-0.4,-0.15));
#16405=CARTESIAN_POINT('',(-0.0866025403784438,-0.64,-0.15));
#16406=CARTESIAN_POINT('',(-0.0866025403784438,-0.4,-0.15));
#16407=CARTESIAN_POINT('',(0.0866025403784439,-0.64,-0.15));
#16408=CARTESIAN_POINT('Origin',(-0.173205080756888,-0.4,-2.77555756156289E-17));
#16409=CARTESIAN_POINT('',(-0.173205080756888,-0.4,-2.12115047744981E-17));
#16410=CARTESIAN_POINT('',(-0.0866025403784438,-0.4,-0.15));
#16411=CARTESIAN_POINT('',(-0.173205080756888,-0.64,-2.77555756156289E-17));
#16412=CARTESIAN_POINT('',(-0.173205080756888,-0.4,-2.12115047744981E-17));
#16413=CARTESIAN_POINT('',(-0.0866025403784438,-0.64,-0.15));
#16414=CARTESIAN_POINT('Origin',(-0.0866025403784439,-0.4,0.15));
#16415=CARTESIAN_POINT('',(-0.0866025403784439,-0.4,0.15));
#16416=CARTESIAN_POINT('',(-0.173205080756888,-0.4,-2.12115047744981E-17));
#16417=CARTESIAN_POINT('',(-0.0866025403784439,-0.64,0.15));
#16418=CARTESIAN_POINT('',(-0.0866025403784439,-0.4,0.15));
#16419=CARTESIAN_POINT('',(-0.173205080756888,-0.64,-2.12115047744981E-17));
#16420=CARTESIAN_POINT('Origin',(0.0866025403784439,-0.4,0.15));
#16421=CARTESIAN_POINT('',(0.0866025403784439,-0.4,0.15));
#16422=CARTESIAN_POINT('',(-0.0866025403784439,-0.4,0.15));
#16423=CARTESIAN_POINT('',(0.0866025403784439,-0.64,0.15));
#16424=CARTESIAN_POINT('',(0.0866025403784439,-0.4,0.15));
#16425=CARTESIAN_POINT('',(-0.0866025403784439,-0.64,0.15));
#16426=CARTESIAN_POINT('Origin',(0.173205080756888,-0.4,0.));
#16427=CARTESIAN_POINT('',(0.0866025403784439,-0.4,0.15));
#16428=CARTESIAN_POINT('',(0.0866025403784439,-0.64,0.15));
#16429=CARTESIAN_POINT('Origin',(0.,-0.4,-2.77555756156289E-17));
#16430=CARTESIAN_POINT('Origin',(0.,-0.64,-2.77555756156289E-17));
#16431=CARTESIAN_POINT('',(0.,0.,0.));
#16432=CARTESIAN_POINT('',(0.,0.,0.));
#16433=CARTESIAN_POINT('',(0.,0.,0.));
#16434=CARTESIAN_POINT('',(0.,0.,0.));
#16435=CARTESIAN_POINT('',(0.,0.,0.));
#16436=CARTESIAN_POINT('',(0.,0.,0.));
#16437=CARTESIAN_POINT('',(0.,0.,0.));
#16438=CARTESIAN_POINT('',(0.,0.,0.));
#16439=CARTESIAN_POINT('',(0.,0.,0.));
#16440=CARTESIAN_POINT('',(0.,0.,0.));
#16441=CARTESIAN_POINT('',(0.,0.,0.));
#16442=CARTESIAN_POINT('',(0.,0.,0.));
#16443=CARTESIAN_POINT('',(0.,0.,0.));
#16444=CARTESIAN_POINT('',(0.,0.,0.));
#16445=CARTESIAN_POINT('',(0.,0.,0.));
#16446=CARTESIAN_POINT('',(0.,0.,0.));
#16447=CARTESIAN_POINT('',(0.,0.,0.));
#16448=CARTESIAN_POINT('',(0.,0.,0.));
#16449=CARTESIAN_POINT('',(0.,0.,0.));
#16450=CARTESIAN_POINT('',(0.,0.,0.));
#16451=CARTESIAN_POINT('',(0.,0.,0.));
#16452=CARTESIAN_POINT('',(0.,0.,0.));
#16453=CARTESIAN_POINT('',(0.,0.,0.));
#16454=CARTESIAN_POINT('',(-2.8,1.2,2.));
#16455=CARTESIAN_POINT('',(-2.8,5.3,2.));
#16456=CARTESIAN_POINT('',(8.3,1.2,2.));
#16457=CARTESIAN_POINT('',(8.3,5.3,2.));
#16458=CARTESIAN_POINT('',(-2.9,-7.,1.8));
#16459=CARTESIAN_POINT('',(2.9,-7.,1.8));
#16460=CARTESIAN_POINT('',(0.,-7.,7.));
#16461=CARTESIAN_POINT('',(1.48492424049175,-8.,8.48492424049175));
#16462=CARTESIAN_POINT('',(-1.48492424049175,-8.,8.48492424049175));
#16463=CARTESIAN_POINT('',(-1.48492424049175,-8.,5.51507575950825));
#16464=CARTESIAN_POINT('',(1.48492424049175,-8.,5.51507575950825));
#16465=CARTESIAN_POINT('',(1.48492424049175,-6.,8.48492424049175));
#16466=CARTESIAN_POINT('',(-1.48492424049175,-6.,8.48492424049175));
#16467=CARTESIAN_POINT('',(-1.48492424049175,-6.,5.51507575950825));
#16468=CARTESIAN_POINT('',(1.48492424049175,-6.,5.51507575950825));
#16469=CARTESIAN_POINT('',(-2.9,-4.,1.8));
#16470=CARTESIAN_POINT('',(2.9,-4.,1.8));
#16471=CARTESIAN_POINT('',(0.,-4.,7.));
#16472=CARTESIAN_POINT('',(1.48492424049175,-5.,8.48492424049175));
#16473=CARTESIAN_POINT('',(-1.48492424049175,-5.,8.48492424049175));
#16474=CARTESIAN_POINT('',(-1.48492424049175,-5.,5.51507575950825));
#16475=CARTESIAN_POINT('',(1.48492424049175,-5.,5.51507575950825));
#16476=CARTESIAN_POINT('',(1.48492424049175,-3.,8.48492424049175));
#16477=CARTESIAN_POINT('',(-1.48492424049175,-3.,8.48492424049175));
#16478=CARTESIAN_POINT('',(-1.48492424049175,-3.,5.51507575950825));
#16479=CARTESIAN_POINT('',(1.48492424049175,-3.,5.51507575950825));
#16480=CARTESIAN_POINT('',(-1.7,1.5,2.8));
#16481=CARTESIAN_POINT('',(1.1,4.5,2.8));
#16482=CARTESIAN_POINT('',(-0.3,3.,7.));
#16483=CARTESIAN_POINT('',(-1.3,4.48492424049175,8.48492424049175));
#16484=CARTESIAN_POINT('',(-1.3,1.51507575950825,8.48492424049175));
#16485=CARTESIAN_POINT('',(-1.3,1.51507575950825,5.51507575950825));
#16486=CARTESIAN_POINT('',(-1.3,4.48492424049175,5.51507575950825));
#16487=CARTESIAN_POINT('',(0.7,4.48492424049175,8.48492424049175));
#16488=CARTESIAN_POINT('',(0.7,1.51507575950825,8.48492424049175));
#16489=CARTESIAN_POINT('',(0.7,1.51507575950825,5.51507575950825));
#16490=CARTESIAN_POINT('',(0.7,4.48492424049175,5.51507575950825));
#16491=CARTESIAN_POINT('',(4.1,1.5,2.8));
#16492=CARTESIAN_POINT('',(6.9,4.5,2.8));
#16493=CARTESIAN_POINT('',(5.5,3.,7.));
#16494=CARTESIAN_POINT('',(4.5,4.48492424049175,8.48492424049175));
#16495=CARTESIAN_POINT('',(4.5,1.51507575950825,8.48492424049175));
#16496=CARTESIAN_POINT('',(4.5,1.51507575950825,5.51507575950825));
#16497=CARTESIAN_POINT('',(4.5,4.48492424049175,5.51507575950825));
#16498=CARTESIAN_POINT('',(6.5,4.48492424049175,8.48492424049175));
#16499=CARTESIAN_POINT('',(6.5,1.51507575950825,8.48492424049175));
#16500=CARTESIAN_POINT('',(6.5,1.51507575950825,5.51507575950825));
#16501=CARTESIAN_POINT('',(6.5,4.48492424049175,5.51507575950825));
#16502=CARTESIAN_POINT('',(-1.5,8.5,1.6));
#16503=CARTESIAN_POINT('',(7.,8.5,1.6));
#16504=CARTESIAN_POINT('',(-0.3,9.9,4.));
#16505=CARTESIAN_POINT('',(-0.3,9.,4.));
#16506=CARTESIAN_POINT('',(5.5,9.9,4.));
#16507=CARTESIAN_POINT('',(5.5,9.,4.));
#16508=CARTESIAN_POINT('',(0.,0.,0.));
#16509=CARTESIAN_POINT('',(0.,0.,0.));
#16510=CARTESIAN_POINT('Origin',(1.5,3.2,6.3));
#16511=CARTESIAN_POINT('',(2.9,3.2,6.43431457505076));
#16512=CARTESIAN_POINT('',(1.5,3.2,6.43431457505076));
#16513=CARTESIAN_POINT('',(-2.5,3.2,6.43431457505076));
#16514=CARTESIAN_POINT('',(2.9,3.2,6.65));
#16515=CARTESIAN_POINT('',(2.9,3.2,6.3));
#16516=CARTESIAN_POINT('',(1.5,3.2,6.65));
#16517=CARTESIAN_POINT('',(1.5,3.2,6.65));
#16518=CARTESIAN_POINT('',(1.5,3.2,6.3));
#16519=CARTESIAN_POINT('Origin',(1.5,3.,6.475));
#16520=CARTESIAN_POINT('',(1.5,2.8,6.43431457505076));
#16521=CARTESIAN_POINT('Origin',(1.5,3.,7.));
#16522=CARTESIAN_POINT('',(1.5,2.8,6.65));
#16523=CARTESIAN_POINT('',(1.5,3.2,6.65));
#16524=CARTESIAN_POINT('',(1.5,2.8,6.65));
#16525=CARTESIAN_POINT('Origin',(1.5,3.2,6.65));
#16526=CARTESIAN_POINT('',(2.9,2.8,6.65));
#16527=CARTESIAN_POINT('',(2.9,3.2,6.65));
#16528=CARTESIAN_POINT('',(1.5,2.8,6.65));
#16529=CARTESIAN_POINT('Origin',(1.5,2.8,6.65));
#16530=CARTESIAN_POINT('',(2.9,2.8,6.43431457505076));
#16531=CARTESIAN_POINT('',(-2.5,2.8,6.43431457505076));
#16532=CARTESIAN_POINT('',(2.9,2.8,6.65));
#16533=CARTESIAN_POINT('Origin',(2.9,3.,6.475));
#16534=CARTESIAN_POINT('Origin',(2.9,3.,7.));
#16535=CARTESIAN_POINT('Origin',(1.2,3.,7.));
#16536=CARTESIAN_POINT('',(1.2,3.,7.8));
#16537=CARTESIAN_POINT('Origin',(1.2,3.,7.));
#16538=CARTESIAN_POINT('',(1.2,3.,7.6));
#16539=CARTESIAN_POINT('Origin',(1.2,3.,7.));
#16540=CARTESIAN_POINT('Origin',(0.2,3.,7.));
#16541=CARTESIAN_POINT('',(0.2,3.,7.8));
#16542=CARTESIAN_POINT('Origin',(0.2,3.,7.));
#16543=CARTESIAN_POINT('',(0.2,3.,7.6));
#16544=CARTESIAN_POINT('Origin',(0.2,3.,7.));
#16545=CARTESIAN_POINT('Origin',(0.2,3.,7.));
#16546=CARTESIAN_POINT('',(0.2,3.,7.8));
#16547=CARTESIAN_POINT('Origin',(-2.5,3.,7.));
#16548=CARTESIAN_POINT('',(-2.5,3.,7.6));
#16549=CARTESIAN_POINT('',(-2.5,3.,7.6));
#16550=CARTESIAN_POINT('Origin',(-2.5,3.,7.));
#16551=CARTESIAN_POINT('Origin',(-2.5,3.,7.));
#16552=CARTESIAN_POINT('',(7.5,3.,7.6));
#16553=CARTESIAN_POINT('Origin',(7.5,3.,7.));
#16554=CARTESIAN_POINT('',(-2.5,3.,7.6));
#16555=CARTESIAN_POINT('Origin',(7.5,3.,7.));
#16556=CARTESIAN_POINT('Origin',(-2.5,3.,7.));
#16557=CARTESIAN_POINT('',(0.,0.,0.));
#16558=CARTESIAN_POINT('Origin',(1.1,3.2,6.22));
#16559=CARTESIAN_POINT('',(1.2,3.2,6.22));
#16560=CARTESIAN_POINT('',(1.2,3.2,6.43431457505076));
#16561=CARTESIAN_POINT('',(1.2,3.2,6.61));
#16562=CARTESIAN_POINT('',(3.2,3.2,6.22));
#16563=CARTESIAN_POINT('',(1.1,3.2,6.22));
#16564=CARTESIAN_POINT('',(3.2,3.2,6.43431457505076));
#16565=CARTESIAN_POINT('',(3.2,3.2,6.61));
#16566=CARTESIAN_POINT('',(1.2,3.2,6.43431457505076));
#16567=CARTESIAN_POINT('Origin',(1.1,2.8,6.22));
#16568=CARTESIAN_POINT('',(1.2,2.8,6.22));
#16569=CARTESIAN_POINT('',(1.2,2.9,6.22));
#16570=CARTESIAN_POINT('',(3.2,2.8,6.22));
#16571=CARTESIAN_POINT('',(1.1,2.8,6.22));
#16572=CARTESIAN_POINT('',(3.2,2.9,6.22));
#16573=CARTESIAN_POINT('Origin',(1.1,2.8,7.));
#16574=CARTESIAN_POINT('',(1.2,2.8,6.43431457505076));
#16575=CARTESIAN_POINT('',(1.2,2.8,7.));
#16576=CARTESIAN_POINT('',(3.2,2.8,6.43431457505076));
#16577=CARTESIAN_POINT('',(1.2,2.8,6.43431457505076));
#16578=CARTESIAN_POINT('',(3.2,2.8,7.));
#16579=CARTESIAN_POINT('Origin',(3.2,3.,7.));
#16580=CARTESIAN_POINT('',(3.2,3.,8.2));
#16581=CARTESIAN_POINT('Origin',(3.2,3.,7.));
#16582=CARTESIAN_POINT('Origin',(3.2,3.,7.));
#16583=CARTESIAN_POINT('Origin',(1.2,3.,7.));
#16584=CARTESIAN_POINT('Origin',(1.2,3.,7.));
#16585=CARTESIAN_POINT('Origin',(1.8,3.,7.));
#16586=CARTESIAN_POINT('',(1.8,3.,9.9));
#16587=CARTESIAN_POINT('Origin',(1.8,3.,7.));
#16588=CARTESIAN_POINT('',(1.8,3.,8.2));
#16589=CARTESIAN_POINT('Origin',(1.8,3.,7.));
#16590=CARTESIAN_POINT('Origin',(1.2,3.,7.));
#16591=CARTESIAN_POINT('',(1.2,3.,9.9));
#16592=CARTESIAN_POINT('',(1.2,3.,9.9));
#16593=CARTESIAN_POINT('Origin',(1.2,3.,7.));
#16594=CARTESIAN_POINT('Origin',(1.2,3.,7.));
#16595=CARTESIAN_POINT('',(1.2,3.,8.2));
#16596=CARTESIAN_POINT('Origin',(1.2,3.,7.));
#16597=CARTESIAN_POINT('',(0.,0.,0.));
#16598=CARTESIAN_POINT('Origin',(1.2,3.,7.));
#16599=CARTESIAN_POINT('',(1.8,3.,9.9));
#16600=CARTESIAN_POINT('Origin',(1.8,3.,7.));
#16601=CARTESIAN_POINT('',(1.2,3.,9.9));
#16602=CARTESIAN_POINT('',(1.2,3.,9.9));
#16603=CARTESIAN_POINT('Origin',(1.2,3.,7.));
#16604=CARTESIAN_POINT('Origin',(1.2,3.,7.));
#16605=CARTESIAN_POINT('',(1.8,3.,10.));
#16606=CARTESIAN_POINT('Origin',(1.8,3.,7.));
#16607=CARTESIAN_POINT('',(1.2,3.,10.));
#16608=CARTESIAN_POINT('',(1.2,3.,10.));
#16609=CARTESIAN_POINT('Origin',(1.2,3.,7.));
#16610=CARTESIAN_POINT('Origin',(1.8,3.,7.));
#16611=CARTESIAN_POINT('Origin',(1.2,3.,7.));
#16612=CARTESIAN_POINT('',(0.,0.,0.));
#16613=CARTESIAN_POINT('Origin',(3.2,3.,7.));
#16614=CARTESIAN_POINT('',(5.,3.,7.605));
#16615=CARTESIAN_POINT('Origin',(5.,3.,7.));
#16616=CARTESIAN_POINT('',(3.2,3.,7.605));
#16617=CARTESIAN_POINT('',(3.2,3.,7.605));
#16618=CARTESIAN_POINT('Origin',(3.2,3.,7.));
#16619=CARTESIAN_POINT('Origin',(3.2,3.,7.));
#16620=CARTESIAN_POINT('',(5.,3.,7.8));
#16621=CARTESIAN_POINT('Origin',(5.,3.,7.));
#16622=CARTESIAN_POINT('',(3.2,3.,7.8));
#16623=CARTESIAN_POINT('',(3.2,3.,7.8));
#16624=CARTESIAN_POINT('Origin',(3.2,3.,7.));
#16625=CARTESIAN_POINT('Origin',(5.,3.,7.));
#16626=CARTESIAN_POINT('Origin',(3.2,3.,7.));
#16627=CARTESIAN_POINT('',(0.,0.,0.));
#16628=CARTESIAN_POINT('Origin',(-1.2,3.,7.59));
#16629=CARTESIAN_POINT('',(-1.36178689687364,2.86611572161004,7.59));
#16630=CARTESIAN_POINT('',(-1.03821310312636,2.86611572161004,7.59));
#16631=CARTESIAN_POINT('',(-1.6,2.86611572161004,7.59));
#16632=CARTESIAN_POINT('Origin',(-1.2,3.,7.59));
#16633=CARTESIAN_POINT('Origin',(-1.2,3.,7.59));
#16634=CARTESIAN_POINT('',(-1.36178689687364,3.13388427838996,7.59));
#16635=CARTESIAN_POINT('',(-1.41,3.,7.605));
#16636=CARTESIAN_POINT('Ctrl Pts',(-1.36178689687364,3.13388427838996,7.59));
#16637=CARTESIAN_POINT('Ctrl Pts',(-1.37472116821763,3.1182543952608,7.59354677224418));
#16638=CARTESIAN_POINT('Ctrl Pts',(-1.38579931658744,3.1001097876823,7.59698224789957));
#16639=CARTESIAN_POINT('Ctrl Pts',(-1.40463856105443,3.05482987213252,7.6030741628997));
#16640=CARTESIAN_POINT('Ctrl Pts',(-1.41,3.02660205959229,7.605));
#16641=CARTESIAN_POINT('Ctrl Pts',(-1.41,3.,7.605));
#16642=CARTESIAN_POINT('',(-1.03821310312636,3.13388427838996,7.59));
#16643=CARTESIAN_POINT('Origin',(-1.2,3.,7.59));
#16644=CARTESIAN_POINT('',(-0.99,3.,7.605));
#16645=CARTESIAN_POINT('Ctrl Pts',(-0.99,3.,7.605));
#16646=CARTESIAN_POINT('Ctrl Pts',(-0.99,3.02660205959229,7.605));
#16647=CARTESIAN_POINT('Ctrl Pts',(-0.995361438945571,3.05482987213252,
7.6030741628997));
#16648=CARTESIAN_POINT('Ctrl Pts',(-1.01420068341256,3.1001097876823,7.59698224789957));
#16649=CARTESIAN_POINT('Ctrl Pts',(-1.02527883178237,3.1182543952608,7.59354677224418));
#16650=CARTESIAN_POINT('Ctrl Pts',(-1.03821310312636,3.13388427838996,7.59));
#16651=CARTESIAN_POINT('Ctrl Pts',(-1.03821310312636,2.86611572161004,7.59));
#16652=CARTESIAN_POINT('Ctrl Pts',(-1.02527883178237,2.8817456047392,7.59354677224418));
#16653=CARTESIAN_POINT('Ctrl Pts',(-1.01420068341256,2.8998902123177,7.59698224789957));
#16654=CARTESIAN_POINT('Ctrl Pts',(-0.995361438945571,2.94517012786748,
7.6030741628997));
#16655=CARTESIAN_POINT('Ctrl Pts',(-0.99,2.97339794040771,7.605));
#16656=CARTESIAN_POINT('Ctrl Pts',(-0.99,3.,7.605));
#16657=CARTESIAN_POINT('Ctrl Pts',(-1.41,3.,7.605));
#16658=CARTESIAN_POINT('Ctrl Pts',(-1.41,2.97339794040771,7.605));
#16659=CARTESIAN_POINT('Ctrl Pts',(-1.40463856105443,2.94517012786748,7.6030741628997));
#16660=CARTESIAN_POINT('Ctrl Pts',(-1.38579931658744,2.8998902123177,7.59698224789957));
#16661=CARTESIAN_POINT('Ctrl Pts',(-1.37472116821763,2.8817456047392,7.59354677224418));
#16662=CARTESIAN_POINT('Ctrl Pts',(-1.36178689687364,2.86611572161004,7.59));
#16663=CARTESIAN_POINT('',(-1.41,3.,8.1));
#16664=CARTESIAN_POINT('',(-1.41,3.,7.59));
#16665=CARTESIAN_POINT('',(-1.2,2.79,8.07976849370594));
#16666=CARTESIAN_POINT('Ctrl Pts',(-1.2,2.79,8.07976849370594));
#16667=CARTESIAN_POINT('Ctrl Pts',(-1.22643858813051,2.79,8.07976849370594));
#16668=CARTESIAN_POINT('Ctrl Pts',(-1.25459378125493,2.79529707732902,8.08084015664674));
#16669=CARTESIAN_POINT('Ctrl Pts',(-1.30631344554134,2.81674820319365,8.08468313707126));
#16670=CARTESIAN_POINT('Ctrl Pts',(-1.32988367074114,2.83289882264279,8.08739593054622));
#16671=CARTESIAN_POINT('Ctrl Pts',(-1.36710031461738,2.87011546651904,8.09246633289124));
#16672=CARTESIAN_POINT('Ctrl Pts',(-1.38325161016341,2.89368605924271,8.09515738895358));
#16673=CARTESIAN_POINT('Ctrl Pts',(-1.40470322656974,2.94540699667048,8.09895039220591));
#16674=CARTESIAN_POINT('Ctrl Pts',(-1.41,2.97356263761646,8.1));
#16675=CARTESIAN_POINT('Ctrl Pts',(-1.41,3.,8.1));
#16676=CARTESIAN_POINT('',(-0.99,3.,8.1));
#16677=CARTESIAN_POINT('Ctrl Pts',(-0.99,3.,8.1));
#16678=CARTESIAN_POINT('Ctrl Pts',(-0.99,2.97356263761646,8.1));
#16679=CARTESIAN_POINT('Ctrl Pts',(-0.995296773430262,2.94540699667048,
8.09895039220591));
#16680=CARTESIAN_POINT('Ctrl Pts',(-1.01674838983659,2.89368605924271,8.09515738895358));
#16681=CARTESIAN_POINT('Ctrl Pts',(-1.03289968538261,2.87011546651904,8.09246633289124));
#16682=CARTESIAN_POINT('Ctrl Pts',(-1.07011632925886,2.83289882264279,8.08739593054622));
#16683=CARTESIAN_POINT('Ctrl Pts',(-1.09368655445866,2.81674820319365,8.08468313707126));
#16684=CARTESIAN_POINT('Ctrl Pts',(-1.14540621874507,2.79529707732902,8.08084015664674));
#16685=CARTESIAN_POINT('Ctrl Pts',(-1.17356141186949,2.79,8.07976849370594));
#16686=CARTESIAN_POINT('Ctrl Pts',(-1.2,2.79,8.07976849370594));
#16687=CARTESIAN_POINT('Ctrl Pts',(-1.41,3.,8.1));
#16688=CARTESIAN_POINT('Ctrl Pts',(-1.41,3.02643736238354,8.1));
#16689=CARTESIAN_POINT('Ctrl Pts',(-1.40470322656974,3.05459300332952,8.09895039220591));
#16690=CARTESIAN_POINT('Ctrl Pts',(-1.38325161016341,3.10631394075729,8.09515738895358));
#16691=CARTESIAN_POINT('Ctrl Pts',(-1.36710031461738,3.12988453348096,8.09246633289124));
#16692=CARTESIAN_POINT('Ctrl Pts',(-1.32988367074114,3.16710117735721,8.08739593054622));
#16693=CARTESIAN_POINT('Ctrl Pts',(-1.30631344554134,3.18325179680635,8.08468313707126));
#16694=CARTESIAN_POINT('Ctrl Pts',(-1.25459378125493,3.20470292267098,8.08084015664674));
#16695=CARTESIAN_POINT('Ctrl Pts',(-1.22643858813051,3.21,8.07976849370594));
#16696=CARTESIAN_POINT('Ctrl Pts',(-1.17356141186949,3.21,8.07976849370594));
#16697=CARTESIAN_POINT('Ctrl Pts',(-1.14540621874507,3.20470292267098,8.08084015664674));
#16698=CARTESIAN_POINT('Ctrl Pts',(-1.09368655445866,3.18325179680635,8.08468313707126));
#16699=CARTESIAN_POINT('Ctrl Pts',(-1.07011632925886,3.16710117735721,8.08739593054622));
#16700=CARTESIAN_POINT('Ctrl Pts',(-1.03289968538262,3.12988453348096,8.09246633289124));
#16701=CARTESIAN_POINT('Ctrl Pts',(-1.01674838983659,3.10631394075729,8.09515738895358));
#16702=CARTESIAN_POINT('Ctrl Pts',(-0.995296773430262,3.05459300332952,
8.09895039220591));
#16703=CARTESIAN_POINT('Ctrl Pts',(-0.99,3.02643736238354,8.1));
#16704=CARTESIAN_POINT('Ctrl Pts',(-0.99,3.,8.1));
#16705=CARTESIAN_POINT('Origin',(-1.2,3.,7.59));
#16706=CARTESIAN_POINT('',(-1.6,3.13388427838996,7.59));
#16707=CARTESIAN_POINT('Origin',(-1.6,3.,7.));
#16708=CARTESIAN_POINT('',(-0.8,3.,7.605));
#16709=CARTESIAN_POINT('Origin',(-0.8,3.,7.));
#16710=CARTESIAN_POINT('',(-1.6,3.,7.605));
#16711=CARTESIAN_POINT('',(-1.6,3.,7.605));
#16712=CARTESIAN_POINT('',(-1.6,3.,7.605));
#16713=CARTESIAN_POINT('Origin',(-1.6,3.,7.));
#16714=CARTESIAN_POINT('Origin',(-1.6,3.,7.));
#16715=CARTESIAN_POINT('',(-0.8,3.,8.1));
#16716=CARTESIAN_POINT('Origin',(-0.8,3.,7.));
#16717=CARTESIAN_POINT('',(-1.6,3.,8.1));
#16718=CARTESIAN_POINT('',(-1.6,3.,8.1));
#16719=CARTESIAN_POINT('',(-1.6,3.,8.1));
#16720=CARTESIAN_POINT('Origin',(-1.6,3.,7.));
#16721=CARTESIAN_POINT('Origin',(-0.8,3.,7.));
#16722=CARTESIAN_POINT('Origin',(-1.6,3.,7.));
#16723=CARTESIAN_POINT('',(0.,0.,0.));
#16724=CARTESIAN_POINT('Origin',(6.4,3.,7.59));
#16725=CARTESIAN_POINT('',(6.23821310312636,2.86611572161004,7.59));
#16726=CARTESIAN_POINT('',(6.56178689687364,2.86611572161004,7.59));
#16727=CARTESIAN_POINT('',(6.,2.86611572161004,7.59));
#16728=CARTESIAN_POINT('Origin',(6.4,3.,7.59));
#16729=CARTESIAN_POINT('Origin',(6.4,3.,7.59));
#16730=CARTESIAN_POINT('',(6.23821310312636,3.13388427838996,7.59));
#16731=CARTESIAN_POINT('',(6.19,3.,7.605));
#16732=CARTESIAN_POINT('Ctrl Pts',(6.23821310312637,3.13388427838996,7.59));
#16733=CARTESIAN_POINT('Ctrl Pts',(6.22527883178237,3.1182543952608,7.59354677224418));
#16734=CARTESIAN_POINT('Ctrl Pts',(6.21420068341256,3.1001097876823,7.59698224789957));
#16735=CARTESIAN_POINT('Ctrl Pts',(6.19536143894557,3.05482987213252,7.6030741628997));
#16736=CARTESIAN_POINT('Ctrl Pts',(6.19,3.02660205959229,7.605));
#16737=CARTESIAN_POINT('Ctrl Pts',(6.19,3.,7.605));
#16738=CARTESIAN_POINT('',(6.56178689687364,3.13388427838996,7.59));
#16739=CARTESIAN_POINT('Origin',(6.4,3.,7.59));
#16740=CARTESIAN_POINT('',(6.61,3.,7.605));
#16741=CARTESIAN_POINT('Ctrl Pts',(6.61,3.,7.605));
#16742=CARTESIAN_POINT('Ctrl Pts',(6.61,3.02660205959229,7.605));
#16743=CARTESIAN_POINT('Ctrl Pts',(6.60463856105443,3.05482987213252,7.6030741628997));
#16744=CARTESIAN_POINT('Ctrl Pts',(6.58579931658744,3.1001097876823,7.59698224789957));
#16745=CARTESIAN_POINT('Ctrl Pts',(6.57472116821763,3.1182543952608,7.59354677224418));
#16746=CARTESIAN_POINT('Ctrl Pts',(6.56178689687364,3.13388427838996,7.59));
#16747=CARTESIAN_POINT('Ctrl Pts',(6.56178689687364,2.86611572161004,7.59));
#16748=CARTESIAN_POINT('Ctrl Pts',(6.57472116821763,2.8817456047392,7.59354677224418));
#16749=CARTESIAN_POINT('Ctrl Pts',(6.58579931658744,2.8998902123177,7.59698224789957));
#16750=CARTESIAN_POINT('Ctrl Pts',(6.60463856105443,2.94517012786748,7.6030741628997));
#16751=CARTESIAN_POINT('Ctrl Pts',(6.61,2.97339794040771,7.605));
#16752=CARTESIAN_POINT('Ctrl Pts',(6.61,3.,7.605));
#16753=CARTESIAN_POINT('Ctrl Pts',(6.19,3.,7.605));
#16754=CARTESIAN_POINT('Ctrl Pts',(6.19,2.97339794040771,7.605));
#16755=CARTESIAN_POINT('Ctrl Pts',(6.19536143894557,2.94517012786748,7.6030741628997));
#16756=CARTESIAN_POINT('Ctrl Pts',(6.21420068341256,2.8998902123177,7.59698224789957));
#16757=CARTESIAN_POINT('Ctrl Pts',(6.22527883178237,2.8817456047392,7.59354677224418));
#16758=CARTESIAN_POINT('Ctrl Pts',(6.23821310312636,2.86611572161004,7.59));
#16759=CARTESIAN_POINT('',(6.19,3.,8.1));
#16760=CARTESIAN_POINT('',(6.19,3.,7.59));
#16761=CARTESIAN_POINT('',(6.4,2.79,8.07976849370594));
#16762=CARTESIAN_POINT('Ctrl Pts',(6.4,2.79,8.07976849370594));
#16763=CARTESIAN_POINT('Ctrl Pts',(6.37356141186949,2.79,8.07976849370594));
#16764=CARTESIAN_POINT('Ctrl Pts',(6.34540621874507,2.79529707732902,8.08084015664674));
#16765=CARTESIAN_POINT('Ctrl Pts',(6.29368655445866,2.81674820319365,8.08468313707126));
#16766=CARTESIAN_POINT('Ctrl Pts',(6.27011632925886,2.83289882264279,8.08739593054622));
#16767=CARTESIAN_POINT('Ctrl Pts',(6.23289968538262,2.87011546651904,8.09246633289124));
#16768=CARTESIAN_POINT('Ctrl Pts',(6.21674838983659,2.89368605924271,8.09515738895358));
#16769=CARTESIAN_POINT('Ctrl Pts',(6.19529677343026,2.94540699667048,8.09895039220591));
#16770=CARTESIAN_POINT('Ctrl Pts',(6.19,2.97356263761647,8.1));
#16771=CARTESIAN_POINT('Ctrl Pts',(6.19,3.,8.1));
#16772=CARTESIAN_POINT('',(6.61,3.,8.1));
#16773=CARTESIAN_POINT('Ctrl Pts',(6.61,3.,8.1));
#16774=CARTESIAN_POINT('Ctrl Pts',(6.61,2.97356263761646,8.1));
#16775=CARTESIAN_POINT('Ctrl Pts',(6.60470322656974,2.94540699667048,8.09895039220591));
#16776=CARTESIAN_POINT('Ctrl Pts',(6.58325161016341,2.89368605924271,8.09515738895358));
#16777=CARTESIAN_POINT('Ctrl Pts',(6.56710031461738,2.87011546651904,8.09246633289124));
#16778=CARTESIAN_POINT('Ctrl Pts',(6.52988367074114,2.83289882264279,8.08739593054622));
#16779=CARTESIAN_POINT('Ctrl Pts',(6.50631344554134,2.81674820319365,8.08468313707126));
#16780=CARTESIAN_POINT('Ctrl Pts',(6.45459378125493,2.79529707732902,8.08084015664674));
#16781=CARTESIAN_POINT('Ctrl Pts',(6.42643858813051,2.79,8.07976849370594));
#16782=CARTESIAN_POINT('Ctrl Pts',(6.4,2.79,8.07976849370594));
#16783=CARTESIAN_POINT('Ctrl Pts',(6.19,3.,8.1));
#16784=CARTESIAN_POINT('Ctrl Pts',(6.19,3.02643736238353,8.1));
#16785=CARTESIAN_POINT('Ctrl Pts',(6.19529677343026,3.05459300332952,8.09895039220591));
#16786=CARTESIAN_POINT('Ctrl Pts',(6.21674838983659,3.10631394075729,8.09515738895358));
#16787=CARTESIAN_POINT('Ctrl Pts',(6.23289968538262,3.12988453348096,8.09246633289124));
#16788=CARTESIAN_POINT('Ctrl Pts',(6.27011632925886,3.16710117735721,8.08739593054622));
#16789=CARTESIAN_POINT('Ctrl Pts',(6.29368655445866,3.18325179680635,8.08468313707126));
#16790=CARTESIAN_POINT('Ctrl Pts',(6.34540621874507,3.20470292267098,8.08084015664674));
#16791=CARTESIAN_POINT('Ctrl Pts',(6.37356141186949,3.21,8.07976849370594));
#16792=CARTESIAN_POINT('Ctrl Pts',(6.42643858813051,3.21,8.07976849370594));
#16793=CARTESIAN_POINT('Ctrl Pts',(6.45459378125493,3.20470292267098,8.08084015664674));
#16794=CARTESIAN_POINT('Ctrl Pts',(6.50631344554134,3.18325179680635,8.08468313707126));
#16795=CARTESIAN_POINT('Ctrl Pts',(6.52988367074114,3.16710117735721,8.08739593054622));
#16796=CARTESIAN_POINT('Ctrl Pts',(6.56710031461738,3.12988453348096,8.09246633289124));
#16797=CARTESIAN_POINT('Ctrl Pts',(6.58325161016341,3.10631394075729,8.09515738895358));
#16798=CARTESIAN_POINT('Ctrl Pts',(6.60470322656974,3.05459300332952,8.09895039220591));
#16799=CARTESIAN_POINT('Ctrl Pts',(6.61,3.02643736238354,8.1));
#16800=CARTESIAN_POINT('Ctrl Pts',(6.61,3.,8.1));
#16801=CARTESIAN_POINT('Origin',(6.4,3.,7.59));
#16802=CARTESIAN_POINT('',(6.,3.13388427838996,7.59));
#16803=CARTESIAN_POINT('Origin',(6.,3.,7.));
#16804=CARTESIAN_POINT('',(6.8,3.,7.605));
#16805=CARTESIAN_POINT('Origin',(6.8,3.,7.));
#16806=CARTESIAN_POINT('',(6.,3.,7.605));
#16807=CARTESIAN_POINT('',(6.,3.,7.605));
#16808=CARTESIAN_POINT('',(6.,3.,7.605));
#16809=CARTESIAN_POINT('Origin',(6.,3.,7.));
#16810=CARTESIAN_POINT('Origin',(6.,3.,7.));
#16811=CARTESIAN_POINT('',(6.8,3.,8.1));
#16812=CARTESIAN_POINT('Origin',(6.8,3.,7.));
#16813=CARTESIAN_POINT('',(6.,3.,8.1));
#16814=CARTESIAN_POINT('',(6.,3.,8.1));
#16815=CARTESIAN_POINT('',(6.,3.,8.1));
#16816=CARTESIAN_POINT('Origin',(6.,3.,7.));
#16817=CARTESIAN_POINT('Origin',(6.8,3.,7.));
#16818=CARTESIAN_POINT('Origin',(6.,3.,7.));
#16819=CARTESIAN_POINT('',(0.,0.,0.));
#16820=CARTESIAN_POINT('Origin',(0.7,0.,0.25));
#16821=CARTESIAN_POINT('',(0.7,0.16,0.4));
#16822=CARTESIAN_POINT('',(0.7,0.2,0.36));
#16823=CARTESIAN_POINT('',(0.7,0.1675,0.3925));
#16824=CARTESIAN_POINT('',(0.7,-0.16,0.4));
#16825=CARTESIAN_POINT('',(0.7,0.,0.4));
#16826=CARTESIAN_POINT('',(0.7,-0.2,0.36));
#16827=CARTESIAN_POINT('',(0.7,-0.1675,0.3925));
#16828=CARTESIAN_POINT('',(0.7,-0.2,0.04));
#16829=CARTESIAN_POINT('',(0.7,-0.2,0.125));
#16830=CARTESIAN_POINT('',(0.7,-0.16,0.));
#16831=CARTESIAN_POINT('',(0.7,-0.1925,0.0325));
#16832=CARTESIAN_POINT('',(0.7,0.16,0.));
#16833=CARTESIAN_POINT('',(0.7,0.,0.));
#16834=CARTESIAN_POINT('',(0.7,0.2,0.04));
#16835=CARTESIAN_POINT('',(0.7,0.1925,0.0325));
#16836=CARTESIAN_POINT('',(0.7,0.2,0.125));
#16837=CARTESIAN_POINT('Origin',(-0.4,-0.18,0.02));
#16838=CARTESIAN_POINT('',(-0.7,-0.2,0.04));
#16839=CARTESIAN_POINT('',(-0.4,-0.2,0.04));
#16840=CARTESIAN_POINT('',(-0.7,-0.16,0.));
#16841=CARTESIAN_POINT('',(-0.7,-0.1925,0.0325));
#16842=CARTESIAN_POINT('',(-0.4,-0.16,0.));
#16843=CARTESIAN_POINT('Origin',(-0.8,-0.2,0.));
#16844=CARTESIAN_POINT('',(-0.7,-0.2,0.36));
#16845=CARTESIAN_POINT('',(-0.4,-0.2,0.36));
#16846=CARTESIAN_POINT('',(-0.7,-0.2,0.125));
#16847=CARTESIAN_POINT('Origin',(-0.4,-0.18,0.38));
#16848=CARTESIAN_POINT('',(-0.7,-0.16,0.4));
#16849=CARTESIAN_POINT('',(-0.4,-0.16,0.4));
#16850=CARTESIAN_POINT('',(-0.7,-0.1675,0.3925));
#16851=CARTESIAN_POINT('Origin',(0.,0.,0.4));
#16852=CARTESIAN_POINT('',(-0.7,0.16,0.4));
#16853=CARTESIAN_POINT('',(0.4,0.16,0.4));
#16854=CARTESIAN_POINT('',(-0.7,0.,0.4));
#16855=CARTESIAN_POINT('Origin',(-0.7,0.,0.25));
#16856=CARTESIAN_POINT('',(-0.7,0.2,0.36));
#16857=CARTESIAN_POINT('',(-0.7,0.1675,0.3925));
#16858=CARTESIAN_POINT('',(-0.7,0.2,0.04));
#16859=CARTESIAN_POINT('',(-0.7,0.2,0.125));
#16860=CARTESIAN_POINT('',(-0.7,0.16,0.));
#16861=CARTESIAN_POINT('',(-0.7,0.1925,0.0325));
#16862=CARTESIAN_POINT('',(-0.7,0.,0.));
#16863=CARTESIAN_POINT('Origin',(0.4,0.18,0.38));
#16864=CARTESIAN_POINT('',(0.4,0.2,0.36));
#16865=CARTESIAN_POINT('Origin',(0.8,0.2,0.));
#16866=CARTESIAN_POINT('',(0.4,0.2,0.04));
#16867=CARTESIAN_POINT('Origin',(0.4,0.18,0.02));
#16868=CARTESIAN_POINT('',(0.4,0.16,0.));
#16869=CARTESIAN_POINT('Origin',(0.,0.,0.));
#16870=CARTESIAN_POINT('',(0.,0.,0.));
#16871=CARTESIAN_POINT('Origin',(0.,-0.5,0.));
#16872=CARTESIAN_POINT('',(-0.24505,-0.5,3.00099698131059E-17));
#16873=CARTESIAN_POINT('Origin',(0.,-0.5,0.));
#16874=CARTESIAN_POINT('Origin',(0.0721687836487032,0.,-0.125));
#16875=CARTESIAN_POINT('',(0.0721687836487032,0.,-0.125));
#16876=CARTESIAN_POINT('',(0.144337567297406,0.,0.));
#16877=CARTESIAN_POINT('',(0.117710979560879,0.,-0.0461186027918559));
#16878=CARTESIAN_POINT('',(0.0721687836487032,-0.25,-0.125));
#16879=CARTESIAN_POINT('',(0.0721687836487032,0.,-0.125));
#16880=CARTESIAN_POINT('',(0.144337567297406,-0.25,0.));
#16881=CARTESIAN_POINT('',(0.144337567297406,-0.25,0.));
#16882=CARTESIAN_POINT('',(0.144337567297406,0.,0.));
#16883=CARTESIAN_POINT('Origin',(-0.0721687836487032,0.,-0.125));
#16884=CARTESIAN_POINT('',(-0.0721687836487032,0.,-0.125));
#16885=CARTESIAN_POINT('',(0.0739156081756484,0.,-0.125));
#16886=CARTESIAN_POINT('',(-0.0721687836487032,-0.25,-0.125));
#16887=CARTESIAN_POINT('',(-0.0721687836487032,0.,-0.125));
#16888=CARTESIAN_POINT('',(0.0721687836487032,-0.25,-0.125));
#16889=CARTESIAN_POINT('Origin',(-0.144337567297406,0.,-4.16333634234434E-17));
#16890=CARTESIAN_POINT('',(-0.144337567297406,0.,-1.76762539787485E-17));
#16891=CARTESIAN_POINT('',(-0.0987953713852306,0.,-0.0788813972081442));
#16892=CARTESIAN_POINT('',(-0.144337567297406,-0.25,-2.77555756156289E-17));
#16893=CARTESIAN_POINT('',(-0.144337567297406,0.,-1.76762539787485E-17));
#16894=CARTESIAN_POINT('',(-0.0721687836487032,-0.25,-0.125));
#16895=CARTESIAN_POINT('Origin',(-0.0721687836487033,0.,0.125));
#16896=CARTESIAN_POINT('',(-0.0721687836487033,0.,0.125));
#16897=CARTESIAN_POINT('',(-0.0627109795608791,0.,0.141381397208144));
#16898=CARTESIAN_POINT('',(-0.0721687836487033,-0.25,0.125));
#16899=CARTESIAN_POINT('',(-0.0721687836487033,0.,0.125));
#16900=CARTESIAN_POINT('',(-0.144337567297406,-0.25,-1.76762539787485E-17));
#16901=CARTESIAN_POINT('Origin',(0.0721687836487032,0.,0.125));
#16902=CARTESIAN_POINT('',(0.0721687836487032,0.,0.125));
#16903=CARTESIAN_POINT('',(0.146084391824352,0.,0.125));
#16904=CARTESIAN_POINT('',(0.0721687836487032,-0.25,0.125));
#16905=CARTESIAN_POINT('',(0.0721687836487032,0.,0.125));
#16906=CARTESIAN_POINT('',(-0.0721687836487033,-0.25,0.125));
#16907=CARTESIAN_POINT('Origin',(0.144337567297406,0.,0.));
#16908=CARTESIAN_POINT('',(0.153795371385231,0.,-0.0163813972081441));
#16909=CARTESIAN_POINT('',(0.0721687836487032,-0.25,0.125));
#16910=CARTESIAN_POINT('Origin',(0.,-0.25,0.));
#16911=CARTESIAN_POINT('Origin',(0.22,0.,0.));
#16912=CARTESIAN_POINT('',(-0.22,-8.67361737988404E-18,-2.69422295812418E-17));
#16913=CARTESIAN_POINT('Origin',(0.,0.,0.));
#16914=CARTESIAN_POINT('Origin',(0.,-0.015,0.));
#16915=CARTESIAN_POINT('',(-0.24505,-0.02505,-3.00099698131059E-17));
#16916=CARTESIAN_POINT('Origin',(0.,-0.02505,0.));
#16917=CARTESIAN_POINT('',(-0.235,-0.015,-2.87791997799628E-17));
#16918=CARTESIAN_POINT('Origin',(0.,-0.3775,0.));
#16919=CARTESIAN_POINT('',(-0.24505,-0.3775,-3.00099698131059E-17));
#16920=CARTESIAN_POINT('',(0.,0.,0.));
#16921=CARTESIAN_POINT('',(0.,0.,0.));
#16922=CARTESIAN_POINT('',(0.,0.,0.));
#16923=CARTESIAN_POINT('',(0.,0.,0.));
#16924=CARTESIAN_POINT('',(0.,0.,0.));
#16925=CARTESIAN_POINT('',(0.,0.,0.));
#16926=CARTESIAN_POINT('',(0.,-7.9,8.1));
#16927=CARTESIAN_POINT('',(0.,-1.1,6.65));
#16928=CARTESIAN_POINT('',(0.,0.199999999999999,7.));
#16929=CARTESIAN_POINT('',(0.,0.,0.));
#16930=CARTESIAN_POINT('',(0.,0.,0.));
#16931=CARTESIAN_POINT('',(0.,0.,0.));
#16932=CARTESIAN_POINT('',(0.,0.,0.));
#16933=CARTESIAN_POINT('',(0.,0.,0.));
#16934=CARTESIAN_POINT('',(0.,0.,0.));
#16935=CARTESIAN_POINT('',(2.2,3.,6.65));
#16936=CARTESIAN_POINT('',(-1.2,3.,8.1));
#16937=CARTESIAN_POINT('',(6.4,3.,8.1));
#16938=CARTESIAN_POINT('',(0.,0.,0.));
#16939=CARTESIAN_POINT('',(0.,0.,0.));
#16940=CARTESIAN_POINT('',(0.,0.,0.));
#16941=UNCERTAINTY_MEASURE_WITH_UNIT(LENGTH_MEASURE(0.001),#17047,
'DISTANCE_ACCURACY_VALUE',
'Maximum model space distance between geometric entities at asserted c
onnectivities');
#16942=UNCERTAINTY_MEASURE_WITH_UNIT(LENGTH_MEASURE(0.001),#17047,
'DISTANCE_ACCURACY_VALUE',
'Maximum model space distance between geometric entities at asserted c
onnectivities');
#16943=UNCERTAINTY_MEASURE_WITH_UNIT(LENGTH_MEASURE(0.001),#17047,
'DISTANCE_ACCURACY_VALUE',
'Maximum model space distance between geometric entities at asserted c
onnectivities');
#16944=UNCERTAINTY_MEASURE_WITH_UNIT(LENGTH_MEASURE(0.001),#17047,
'DISTANCE_ACCURACY_VALUE',
'Maximum model space distance between geometric entities at asserted c
onnectivities');
#16945=UNCERTAINTY_MEASURE_WITH_UNIT(LENGTH_MEASURE(0.001),#17047,
'DISTANCE_ACCURACY_VALUE',
'Maximum model space distance between geometric entities at asserted c
onnectivities');
#16946=UNCERTAINTY_MEASURE_WITH_UNIT(LENGTH_MEASURE(0.001),#17047,
'DISTANCE_ACCURACY_VALUE',
'Maximum model space distance between geometric entities at asserted c
onnectivities');
#16947=UNCERTAINTY_MEASURE_WITH_UNIT(LENGTH_MEASURE(0.001),#17047,
'DISTANCE_ACCURACY_VALUE',
'Maximum model space distance between geometric entities at asserted c
onnectivities');
#16948=UNCERTAINTY_MEASURE_WITH_UNIT(LENGTH_MEASURE(0.001),#17047,
'DISTANCE_ACCURACY_VALUE',
'Maximum model space distance between geometric entities at asserted c
onnectivities');
#16949=UNCERTAINTY_MEASURE_WITH_UNIT(LENGTH_MEASURE(0.001),#17047,
'DISTANCE_ACCURACY_VALUE',
'Maximum model space distance between geometric entities at asserted c
onnectivities');
#16950=UNCERTAINTY_MEASURE_WITH_UNIT(LENGTH_MEASURE(0.001),#17047,
'DISTANCE_ACCURACY_VALUE',
'Maximum model space distance between geometric entities at asserted c
onnectivities');
#16951=UNCERTAINTY_MEASURE_WITH_UNIT(LENGTH_MEASURE(0.001),#17047,
'DISTANCE_ACCURACY_VALUE',
'Maximum model space distance between geometric entities at asserted c
onnectivities');
#16952=UNCERTAINTY_MEASURE_WITH_UNIT(LENGTH_MEASURE(0.001),#17047,
'DISTANCE_ACCURACY_VALUE',
'Maximum model space distance between geometric entities at asserted c
onnectivities');
#16953=UNCERTAINTY_MEASURE_WITH_UNIT(LENGTH_MEASURE(0.001),#17047,
'DISTANCE_ACCURACY_VALUE',
'Maximum model space distance between geometric entities at asserted c
onnectivities');
#16954=UNCERTAINTY_MEASURE_WITH_UNIT(LENGTH_MEASURE(0.001),#17047,
'DISTANCE_ACCURACY_VALUE',
'Maximum model space distance between geometric entities at asserted c
onnectivities');
#16955=UNCERTAINTY_MEASURE_WITH_UNIT(LENGTH_MEASURE(0.001),#17047,
'DISTANCE_ACCURACY_VALUE',
'Maximum model space distance between geometric entities at asserted c
onnectivities');
#16956=UNCERTAINTY_MEASURE_WITH_UNIT(LENGTH_MEASURE(0.001),#17047,
'DISTANCE_ACCURACY_VALUE',
'Maximum model space distance between geometric entities at asserted c
onnectivities');
#16957=UNCERTAINTY_MEASURE_WITH_UNIT(LENGTH_MEASURE(0.001),#17047,
'DISTANCE_ACCURACY_VALUE',
'Maximum model space distance between geometric entities at asserted c
onnectivities');
#16958=UNCERTAINTY_MEASURE_WITH_UNIT(LENGTH_MEASURE(0.001),#17047,
'DISTANCE_ACCURACY_VALUE',
'Maximum model space distance between geometric entities at asserted c
onnectivities');
#16959=UNCERTAINTY_MEASURE_WITH_UNIT(LENGTH_MEASURE(0.001),#17047,
'DISTANCE_ACCURACY_VALUE',
'Maximum model space distance between geometric entities at asserted c
onnectivities');
#16960=UNCERTAINTY_MEASURE_WITH_UNIT(LENGTH_MEASURE(0.001),#17047,
'DISTANCE_ACCURACY_VALUE',
'Maximum model space distance between geometric entities at asserted c
onnectivities');
#16961=UNCERTAINTY_MEASURE_WITH_UNIT(LENGTH_MEASURE(0.001),#17047,
'DISTANCE_ACCURACY_VALUE',
'Maximum model space distance between geometric entities at asserted c
onnectivities');
#16962=UNCERTAINTY_MEASURE_WITH_UNIT(LENGTH_MEASURE(0.001),#17047,
'DISTANCE_ACCURACY_VALUE',
'Maximum model space distance between geometric entities at asserted c
onnectivities');
#16963=UNCERTAINTY_MEASURE_WITH_UNIT(LENGTH_MEASURE(0.001),#17047,
'DISTANCE_ACCURACY_VALUE',
'Maximum model space distance between geometric entities at asserted c
onnectivities');
#16964=UNCERTAINTY_MEASURE_WITH_UNIT(LENGTH_MEASURE(0.001),#17047,
'DISTANCE_ACCURACY_VALUE',
'Maximum model space distance between geometric entities at asserted c
onnectivities');
#16965=UNCERTAINTY_MEASURE_WITH_UNIT(LENGTH_MEASURE(0.001),#17047,
'DISTANCE_ACCURACY_VALUE',
'Maximum model space distance between geometric entities at asserted c
onnectivities');
#16966=UNCERTAINTY_MEASURE_WITH_UNIT(LENGTH_MEASURE(0.001),#17047,
'DISTANCE_ACCURACY_VALUE',
'Maximum model space distance between geometric entities at asserted c
onnectivities');
#16967=UNCERTAINTY_MEASURE_WITH_UNIT(LENGTH_MEASURE(0.001),#17047,
'DISTANCE_ACCURACY_VALUE',
'Maximum model space distance between geometric entities at asserted c
onnectivities');
#16968=UNCERTAINTY_MEASURE_WITH_UNIT(LENGTH_MEASURE(0.001),#17047,
'DISTANCE_ACCURACY_VALUE',
'Maximum model space distance between geometric entities at asserted c
onnectivities');
#16969=UNCERTAINTY_MEASURE_WITH_UNIT(LENGTH_MEASURE(0.001),#17047,
'DISTANCE_ACCURACY_VALUE',
'Maximum model space distance between geometric entities at asserted c
onnectivities');
#16970=UNCERTAINTY_MEASURE_WITH_UNIT(LENGTH_MEASURE(0.001),#17047,
'DISTANCE_ACCURACY_VALUE',
'Maximum model space distance between geometric entities at asserted c
onnectivities');
#16971=UNCERTAINTY_MEASURE_WITH_UNIT(LENGTH_MEASURE(0.001),#17047,
'DISTANCE_ACCURACY_VALUE',
'Maximum model space distance between geometric entities at asserted c
onnectivities');
#16972=UNCERTAINTY_MEASURE_WITH_UNIT(LENGTH_MEASURE(0.001),#17047,
'DISTANCE_ACCURACY_VALUE',
'Maximum model space distance between geometric entities at asserted c
onnectivities');
#16973=UNCERTAINTY_MEASURE_WITH_UNIT(LENGTH_MEASURE(0.001),#17047,
'DISTANCE_ACCURACY_VALUE',
'Maximum model space distance between geometric entities at asserted c
onnectivities');
#16974=UNCERTAINTY_MEASURE_WITH_UNIT(LENGTH_MEASURE(0.001),#17047,
'DISTANCE_ACCURACY_VALUE',
'Maximum model space distance between geometric entities at asserted c
onnectivities');
#16975=UNCERTAINTY_MEASURE_WITH_UNIT(LENGTH_MEASURE(0.001),#17047,
'DISTANCE_ACCURACY_VALUE',
'Maximum model space distance between geometric entities at asserted c
onnectivities');
#16976=UNCERTAINTY_MEASURE_WITH_UNIT(LENGTH_MEASURE(0.001),#17047,
'DISTANCE_ACCURACY_VALUE',
'Maximum model space distance between geometric entities at asserted c
onnectivities');
#16977=UNCERTAINTY_MEASURE_WITH_UNIT(LENGTH_MEASURE(0.001),#17047,
'DISTANCE_ACCURACY_VALUE',
'Maximum model space distance between geometric entities at asserted c
onnectivities');
#16978=UNCERTAINTY_MEASURE_WITH_UNIT(LENGTH_MEASURE(0.001),#17047,
'DISTANCE_ACCURACY_VALUE',
'Maximum model space distance between geometric entities at asserted c
onnectivities');
#16979=UNCERTAINTY_MEASURE_WITH_UNIT(LENGTH_MEASURE(0.001),#17047,
'DISTANCE_ACCURACY_VALUE',
'Maximum model space distance between geometric entities at asserted c
onnectivities');
#16980=UNCERTAINTY_MEASURE_WITH_UNIT(LENGTH_MEASURE(0.001),#17047,
'DISTANCE_ACCURACY_VALUE',
'Maximum model space distance between geometric entities at asserted c
onnectivities');
#16981=UNCERTAINTY_MEASURE_WITH_UNIT(LENGTH_MEASURE(0.001),#17047,
'DISTANCE_ACCURACY_VALUE',
'Maximum model space distance between geometric entities at asserted c
onnectivities');
#16982=UNCERTAINTY_MEASURE_WITH_UNIT(LENGTH_MEASURE(0.001),#17047,
'DISTANCE_ACCURACY_VALUE',
'Maximum model space distance between geometric entities at asserted c
onnectivities');
#16983=UNCERTAINTY_MEASURE_WITH_UNIT(LENGTH_MEASURE(0.001),#17047,
'DISTANCE_ACCURACY_VALUE',
'Maximum model space distance between geometric entities at asserted c
onnectivities');
#16984=UNCERTAINTY_MEASURE_WITH_UNIT(LENGTH_MEASURE(0.001),#17047,
'DISTANCE_ACCURACY_VALUE',
'Maximum model space distance between geometric entities at asserted c
onnectivities');
#16985=UNCERTAINTY_MEASURE_WITH_UNIT(LENGTH_MEASURE(0.001),#17047,
'DISTANCE_ACCURACY_VALUE',
'Maximum model space distance between geometric entities at asserted c
onnectivities');
#16986=UNCERTAINTY_MEASURE_WITH_UNIT(LENGTH_MEASURE(0.001),#17047,
'DISTANCE_ACCURACY_VALUE',
'Maximum model space distance between geometric entities at asserted c
onnectivities');
#16987=UNCERTAINTY_MEASURE_WITH_UNIT(LENGTH_MEASURE(0.001),#17047,
'DISTANCE_ACCURACY_VALUE',
'Maximum model space distance between geometric entities at asserted c
onnectivities');
#16988=UNCERTAINTY_MEASURE_WITH_UNIT(LENGTH_MEASURE(0.001),#17047,
'DISTANCE_ACCURACY_VALUE',
'Maximum model space distance between geometric entities at asserted c
onnectivities');
#16989=UNCERTAINTY_MEASURE_WITH_UNIT(LENGTH_MEASURE(0.001),#17047,
'DISTANCE_ACCURACY_VALUE',
'Maximum model space distance between geometric entities at asserted c
onnectivities');
#16990=UNCERTAINTY_MEASURE_WITH_UNIT(LENGTH_MEASURE(0.001),#17047,
'DISTANCE_ACCURACY_VALUE',
'Maximum model space distance between geometric entities at asserted c
onnectivities');
#16991=UNCERTAINTY_MEASURE_WITH_UNIT(LENGTH_MEASURE(0.001),#17047,
'DISTANCE_ACCURACY_VALUE',
'Maximum model space distance between geometric entities at asserted c
onnectivities');
#16992=UNCERTAINTY_MEASURE_WITH_UNIT(LENGTH_MEASURE(0.001),#17047,
'DISTANCE_ACCURACY_VALUE',
'Maximum model space distance between geometric entities at asserted c
onnectivities');
#16993=UNCERTAINTY_MEASURE_WITH_UNIT(LENGTH_MEASURE(0.001),#17047,
'DISTANCE_ACCURACY_VALUE',
'Maximum model space distance between geometric entities at asserted c
onnectivities');
#16994=(
GEOMETRIC_REPRESENTATION_CONTEXT(3)
GLOBAL_UNCERTAINTY_ASSIGNED_CONTEXT((#16941))
GLOBAL_UNIT_ASSIGNED_CONTEXT((#17047,#17049,#17050))
REPRESENTATION_CONTEXT('','3D')
);
#16995=(
GEOMETRIC_REPRESENTATION_CONTEXT(3)
GLOBAL_UNCERTAINTY_ASSIGNED_CONTEXT((#16942))
GLOBAL_UNIT_ASSIGNED_CONTEXT((#17047,#17049,#17050))
REPRESENTATION_CONTEXT('','3D')
);
#16996=(
GEOMETRIC_REPRESENTATION_CONTEXT(3)
GLOBAL_UNCERTAINTY_ASSIGNED_CONTEXT((#16943))
GLOBAL_UNIT_ASSIGNED_CONTEXT((#17047,#17049,#17050))
REPRESENTATION_CONTEXT('','3D')
);
#16997=(
GEOMETRIC_REPRESENTATION_CONTEXT(3)
GLOBAL_UNCERTAINTY_ASSIGNED_CONTEXT((#16944))
GLOBAL_UNIT_ASSIGNED_CONTEXT((#17047,#17049,#17050))
REPRESENTATION_CONTEXT('','3D')
);
#16998=(
GEOMETRIC_REPRESENTATION_CONTEXT(3)
GLOBAL_UNCERTAINTY_ASSIGNED_CONTEXT((#16945))
GLOBAL_UNIT_ASSIGNED_CONTEXT((#17047,#17049,#17050))
REPRESENTATION_CONTEXT('','3D')
);
#16999=(
GEOMETRIC_REPRESENTATION_CONTEXT(3)
GLOBAL_UNCERTAINTY_ASSIGNED_CONTEXT((#16946))
GLOBAL_UNIT_ASSIGNED_CONTEXT((#17047,#17049,#17050))
REPRESENTATION_CONTEXT('','3D')
);
#17000=(
GEOMETRIC_REPRESENTATION_CONTEXT(3)
GLOBAL_UNCERTAINTY_ASSIGNED_CONTEXT((#16947))
GLOBAL_UNIT_ASSIGNED_CONTEXT((#17047,#17049,#17050))
REPRESENTATION_CONTEXT('','3D')
);
#17001=(
GEOMETRIC_REPRESENTATION_CONTEXT(3)
GLOBAL_UNCERTAINTY_ASSIGNED_CONTEXT((#16948))
GLOBAL_UNIT_ASSIGNED_CONTEXT((#17047,#17049,#17050))
REPRESENTATION_CONTEXT('','3D')
);
#17002=(
GEOMETRIC_REPRESENTATION_CONTEXT(3)
GLOBAL_UNCERTAINTY_ASSIGNED_CONTEXT((#16949))
GLOBAL_UNIT_ASSIGNED_CONTEXT((#17047,#17049,#17050))
REPRESENTATION_CONTEXT('','3D')
);
#17003=(
GEOMETRIC_REPRESENTATION_CONTEXT(3)
GLOBAL_UNCERTAINTY_ASSIGNED_CONTEXT((#16950))
GLOBAL_UNIT_ASSIGNED_CONTEXT((#17047,#17049,#17050))
REPRESENTATION_CONTEXT('','3D')
);
#17004=(
GEOMETRIC_REPRESENTATION_CONTEXT(3)
GLOBAL_UNCERTAINTY_ASSIGNED_CONTEXT((#16951))
GLOBAL_UNIT_ASSIGNED_CONTEXT((#17047,#17049,#17050))
REPRESENTATION_CONTEXT('','3D')
);
#17005=(
GEOMETRIC_REPRESENTATION_CONTEXT(3)
GLOBAL_UNCERTAINTY_ASSIGNED_CONTEXT((#16952))
GLOBAL_UNIT_ASSIGNED_CONTEXT((#17047,#17049,#17050))
REPRESENTATION_CONTEXT('','3D')
);
#17006=(
GEOMETRIC_REPRESENTATION_CONTEXT(3)
GLOBAL_UNCERTAINTY_ASSIGNED_CONTEXT((#16953))
GLOBAL_UNIT_ASSIGNED_CONTEXT((#17047,#17049,#17050))
REPRESENTATION_CONTEXT('','3D')
);
#17007=(
GEOMETRIC_REPRESENTATION_CONTEXT(3)
GLOBAL_UNCERTAINTY_ASSIGNED_CONTEXT((#16954))
GLOBAL_UNIT_ASSIGNED_CONTEXT((#17047,#17049,#17050))
REPRESENTATION_CONTEXT('','3D')
);
#17008=(
GEOMETRIC_REPRESENTATION_CONTEXT(3)
GLOBAL_UNCERTAINTY_ASSIGNED_CONTEXT((#16955))
GLOBAL_UNIT_ASSIGNED_CONTEXT((#17047,#17049,#17050))
REPRESENTATION_CONTEXT('','3D')
);
#17009=(
GEOMETRIC_REPRESENTATION_CONTEXT(3)
GLOBAL_UNCERTAINTY_ASSIGNED_CONTEXT((#16956))
GLOBAL_UNIT_ASSIGNED_CONTEXT((#17047,#17049,#17050))
REPRESENTATION_CONTEXT('','3D')
);
#17010=(
GEOMETRIC_REPRESENTATION_CONTEXT(3)
GLOBAL_UNCERTAINTY_ASSIGNED_CONTEXT((#16957))
GLOBAL_UNIT_ASSIGNED_CONTEXT((#17047,#17049,#17050))
REPRESENTATION_CONTEXT('','3D')
);
#17011=(
GEOMETRIC_REPRESENTATION_CONTEXT(3)
GLOBAL_UNCERTAINTY_ASSIGNED_CONTEXT((#16958))
GLOBAL_UNIT_ASSIGNED_CONTEXT((#17047,#17049,#17050))
REPRESENTATION_CONTEXT('','3D')
);
#17012=(
GEOMETRIC_REPRESENTATION_CONTEXT(3)
GLOBAL_UNCERTAINTY_ASSIGNED_CONTEXT((#16959))
GLOBAL_UNIT_ASSIGNED_CONTEXT((#17047,#17049,#17050))
REPRESENTATION_CONTEXT('','3D')
);
#17013=(
GEOMETRIC_REPRESENTATION_CONTEXT(3)
GLOBAL_UNCERTAINTY_ASSIGNED_CONTEXT((#16960))
GLOBAL_UNIT_ASSIGNED_CONTEXT((#17047,#17049,#17050))
REPRESENTATION_CONTEXT('','3D')
);
#17014=(
GEOMETRIC_REPRESENTATION_CONTEXT(3)
GLOBAL_UNCERTAINTY_ASSIGNED_CONTEXT((#16961))
GLOBAL_UNIT_ASSIGNED_CONTEXT((#17047,#17049,#17050))
REPRESENTATION_CONTEXT('','3D')
);
#17015=(
GEOMETRIC_REPRESENTATION_CONTEXT(3)
GLOBAL_UNCERTAINTY_ASSIGNED_CONTEXT((#16962))
GLOBAL_UNIT_ASSIGNED_CONTEXT((#17047,#17049,#17050))
REPRESENTATION_CONTEXT('','3D')
);
#17016=(
GEOMETRIC_REPRESENTATION_CONTEXT(3)
GLOBAL_UNCERTAINTY_ASSIGNED_CONTEXT((#16963))
GLOBAL_UNIT_ASSIGNED_CONTEXT((#17047,#17049,#17050))
REPRESENTATION_CONTEXT('','3D')
);
#17017=(
GEOMETRIC_REPRESENTATION_CONTEXT(3)
GLOBAL_UNCERTAINTY_ASSIGNED_CONTEXT((#16964))
GLOBAL_UNIT_ASSIGNED_CONTEXT((#17047,#17049,#17050))
REPRESENTATION_CONTEXT('','3D')
);
#17018=(
GEOMETRIC_REPRESENTATION_CONTEXT(3)
GLOBAL_UNCERTAINTY_ASSIGNED_CONTEXT((#16965))
GLOBAL_UNIT_ASSIGNED_CONTEXT((#17047,#17049,#17050))
REPRESENTATION_CONTEXT('','3D')
);
#17019=(
GEOMETRIC_REPRESENTATION_CONTEXT(3)
GLOBAL_UNCERTAINTY_ASSIGNED_CONTEXT((#16966))
GLOBAL_UNIT_ASSIGNED_CONTEXT((#17047,#17049,#17050))
REPRESENTATION_CONTEXT('','3D')
);
#17020=(
GEOMETRIC_REPRESENTATION_CONTEXT(3)
GLOBAL_UNCERTAINTY_ASSIGNED_CONTEXT((#16967))
GLOBAL_UNIT_ASSIGNED_CONTEXT((#17047,#17049,#17050))
REPRESENTATION_CONTEXT('','3D')
);
#17021=(
GEOMETRIC_REPRESENTATION_CONTEXT(3)
GLOBAL_UNCERTAINTY_ASSIGNED_CONTEXT((#16968))
GLOBAL_UNIT_ASSIGNED_CONTEXT((#17047,#17049,#17050))
REPRESENTATION_CONTEXT('','3D')
);
#17022=(
GEOMETRIC_REPRESENTATION_CONTEXT(3)
GLOBAL_UNCERTAINTY_ASSIGNED_CONTEXT((#16969))
GLOBAL_UNIT_ASSIGNED_CONTEXT((#17047,#17049,#17050))
REPRESENTATION_CONTEXT('','3D')
);
#17023=(
GEOMETRIC_REPRESENTATION_CONTEXT(3)
GLOBAL_UNCERTAINTY_ASSIGNED_CONTEXT((#16970))
GLOBAL_UNIT_ASSIGNED_CONTEXT((#17047,#17049,#17050))
REPRESENTATION_CONTEXT('','3D')
);
#17024=(
GEOMETRIC_REPRESENTATION_CONTEXT(3)
GLOBAL_UNCERTAINTY_ASSIGNED_CONTEXT((#16971))
GLOBAL_UNIT_ASSIGNED_CONTEXT((#17047,#17049,#17050))
REPRESENTATION_CONTEXT('','3D')
);
#17025=(
GEOMETRIC_REPRESENTATION_CONTEXT(3)
GLOBAL_UNCERTAINTY_ASSIGNED_CONTEXT((#16972))
GLOBAL_UNIT_ASSIGNED_CONTEXT((#17047,#17049,#17050))
REPRESENTATION_CONTEXT('','3D')
);
#17026=(
GEOMETRIC_REPRESENTATION_CONTEXT(3)
GLOBAL_UNCERTAINTY_ASSIGNED_CONTEXT((#16973))
GLOBAL_UNIT_ASSIGNED_CONTEXT((#17047,#17049,#17050))
REPRESENTATION_CONTEXT('','3D')
);
#17027=(
GEOMETRIC_REPRESENTATION_CONTEXT(3)
GLOBAL_UNCERTAINTY_ASSIGNED_CONTEXT((#16974))
GLOBAL_UNIT_ASSIGNED_CONTEXT((#17047,#17049,#17050))
REPRESENTATION_CONTEXT('','3D')
);
#17028=(
GEOMETRIC_REPRESENTATION_CONTEXT(3)
GLOBAL_UNCERTAINTY_ASSIGNED_CONTEXT((#16975))
GLOBAL_UNIT_ASSIGNED_CONTEXT((#17047,#17049,#17050))
REPRESENTATION_CONTEXT('','3D')
);
#17029=(
GEOMETRIC_REPRESENTATION_CONTEXT(3)
GLOBAL_UNCERTAINTY_ASSIGNED_CONTEXT((#16976))
GLOBAL_UNIT_ASSIGNED_CONTEXT((#17047,#17049,#17050))
REPRESENTATION_CONTEXT('','3D')
);
#17030=(
GEOMETRIC_REPRESENTATION_CONTEXT(3)
GLOBAL_UNCERTAINTY_ASSIGNED_CONTEXT((#16977))
GLOBAL_UNIT_ASSIGNED_CONTEXT((#17047,#17049,#17050))
REPRESENTATION_CONTEXT('','3D')
);
#17031=(
GEOMETRIC_REPRESENTATION_CONTEXT(3)
GLOBAL_UNCERTAINTY_ASSIGNED_CONTEXT((#16978))
GLOBAL_UNIT_ASSIGNED_CONTEXT((#17047,#17049,#17050))
REPRESENTATION_CONTEXT('','3D')
);
#17032=(
GEOMETRIC_REPRESENTATION_CONTEXT(3)
GLOBAL_UNCERTAINTY_ASSIGNED_CONTEXT((#16979))
GLOBAL_UNIT_ASSIGNED_CONTEXT((#17047,#17049,#17050))
REPRESENTATION_CONTEXT('','3D')
);
#17033=(
GEOMETRIC_REPRESENTATION_CONTEXT(3)
GLOBAL_UNCERTAINTY_ASSIGNED_CONTEXT((#16980))
GLOBAL_UNIT_ASSIGNED_CONTEXT((#17047,#17049,#17050))
REPRESENTATION_CONTEXT('','3D')
);
#17034=(
GEOMETRIC_REPRESENTATION_CONTEXT(3)
GLOBAL_UNCERTAINTY_ASSIGNED_CONTEXT((#16981))
GLOBAL_UNIT_ASSIGNED_CONTEXT((#17047,#17049,#17050))
REPRESENTATION_CONTEXT('','3D')
);
#17035=(
GEOMETRIC_REPRESENTATION_CONTEXT(3)
GLOBAL_UNCERTAINTY_ASSIGNED_CONTEXT((#16982))
GLOBAL_UNIT_ASSIGNED_CONTEXT((#17047,#17049,#17050))
REPRESENTATION_CONTEXT('','3D')
);
#17036=(
GEOMETRIC_REPRESENTATION_CONTEXT(3)
GLOBAL_UNCERTAINTY_ASSIGNED_CONTEXT((#16983))
GLOBAL_UNIT_ASSIGNED_CONTEXT((#17047,#17049,#17050))
REPRESENTATION_CONTEXT('','3D')
);
#17037=(
GEOMETRIC_REPRESENTATION_CONTEXT(3)
GLOBAL_UNCERTAINTY_ASSIGNED_CONTEXT((#16984))
GLOBAL_UNIT_ASSIGNED_CONTEXT((#17047,#17049,#17050))
REPRESENTATION_CONTEXT('','3D')
);
#17038=(
GEOMETRIC_REPRESENTATION_CONTEXT(3)
GLOBAL_UNCERTAINTY_ASSIGNED_CONTEXT((#16985))
GLOBAL_UNIT_ASSIGNED_CONTEXT((#17047,#17049,#17050))
REPRESENTATION_CONTEXT('','3D')
);
#17039=(
GEOMETRIC_REPRESENTATION_CONTEXT(3)
GLOBAL_UNCERTAINTY_ASSIGNED_CONTEXT((#16986))
GLOBAL_UNIT_ASSIGNED_CONTEXT((#17047,#17049,#17050))
REPRESENTATION_CONTEXT('','3D')
);
#17040=(
GEOMETRIC_REPRESENTATION_CONTEXT(3)
GLOBAL_UNCERTAINTY_ASSIGNED_CONTEXT((#16987))
GLOBAL_UNIT_ASSIGNED_CONTEXT((#17047,#17049,#17050))
REPRESENTATION_CONTEXT('','3D')
);
#17041=(
GEOMETRIC_REPRESENTATION_CONTEXT(3)
GLOBAL_UNCERTAINTY_ASSIGNED_CONTEXT((#16988))
GLOBAL_UNIT_ASSIGNED_CONTEXT((#17047,#17049,#17050))
REPRESENTATION_CONTEXT('','3D')
);
#17042=(
GEOMETRIC_REPRESENTATION_CONTEXT(3)
GLOBAL_UNCERTAINTY_ASSIGNED_CONTEXT((#16989))
GLOBAL_UNIT_ASSIGNED_CONTEXT((#17047,#17049,#17050))
REPRESENTATION_CONTEXT('','3D')
);
#17043=(
GEOMETRIC_REPRESENTATION_CONTEXT(3)
GLOBAL_UNCERTAINTY_ASSIGNED_CONTEXT((#16990))
GLOBAL_UNIT_ASSIGNED_CONTEXT((#17047,#17049,#17050))
REPRESENTATION_CONTEXT('','3D')
);
#17044=(
GEOMETRIC_REPRESENTATION_CONTEXT(3)
GLOBAL_UNCERTAINTY_ASSIGNED_CONTEXT((#16991))
GLOBAL_UNIT_ASSIGNED_CONTEXT((#17047,#17049,#17050))
REPRESENTATION_CONTEXT('','3D')
);
#17045=(
GEOMETRIC_REPRESENTATION_CONTEXT(3)
GLOBAL_UNCERTAINTY_ASSIGNED_CONTEXT((#16992))
GLOBAL_UNIT_ASSIGNED_CONTEXT((#17047,#17049,#17050))
REPRESENTATION_CONTEXT('','3D')
);
#17046=(
GEOMETRIC_REPRESENTATION_CONTEXT(3)
GLOBAL_UNCERTAINTY_ASSIGNED_CONTEXT((#16993))
GLOBAL_UNIT_ASSIGNED_CONTEXT((#17047,#17049,#17050))
REPRESENTATION_CONTEXT('','3D')
);
#17047=(
LENGTH_UNIT()
NAMED_UNIT(*)
SI_UNIT(.CENTI.,.METRE.)
);
#17048=(
LENGTH_UNIT()
NAMED_UNIT(*)
SI_UNIT($,.METRE.)
);
#17049=(
NAMED_UNIT(*)
PLANE_ANGLE_UNIT()
SI_UNIT($,.RADIAN.)
);
#17050=(
NAMED_UNIT(*)
SI_UNIT($,.STERADIAN.)
SOLID_ANGLE_UNIT()
);
#17051=SHAPE_DEFINITION_REPRESENTATION(#17103,#17258);
#17052=SHAPE_DEFINITION_REPRESENTATION(#17104,#17259);
#17053=SHAPE_DEFINITION_REPRESENTATION(#17105,#17260);
#17054=SHAPE_DEFINITION_REPRESENTATION(#17106,#17261);
#17055=SHAPE_DEFINITION_REPRESENTATION(#17107,#17262);
#17056=SHAPE_DEFINITION_REPRESENTATION(#17108,#17263);
#17057=SHAPE_DEFINITION_REPRESENTATION(#17109,#17264);
#17058=SHAPE_DEFINITION_REPRESENTATION(#17110,#17265);
#17059=SHAPE_DEFINITION_REPRESENTATION(#17111,#17266);
#17060=SHAPE_DEFINITION_REPRESENTATION(#17112,#17267);
#17061=SHAPE_DEFINITION_REPRESENTATION(#17113,#17268);
#17062=SHAPE_DEFINITION_REPRESENTATION(#17114,#17269);
#17063=SHAPE_DEFINITION_REPRESENTATION(#17115,#17270);
#17064=SHAPE_DEFINITION_REPRESENTATION(#17116,#17271);
#17065=SHAPE_DEFINITION_REPRESENTATION(#17117,#17272);
#17066=SHAPE_DEFINITION_REPRESENTATION(#17118,#17273);
#17067=SHAPE_DEFINITION_REPRESENTATION(#17119,#17274);
#17068=SHAPE_DEFINITION_REPRESENTATION(#17120,#17275);
#17069=SHAPE_DEFINITION_REPRESENTATION(#17121,#17276);
#17070=SHAPE_DEFINITION_REPRESENTATION(#17122,#17277);
#17071=SHAPE_DEFINITION_REPRESENTATION(#17123,#17278);
#17072=SHAPE_DEFINITION_REPRESENTATION(#17124,#17279);
#17073=SHAPE_DEFINITION_REPRESENTATION(#17125,#17280);
#17074=SHAPE_DEFINITION_REPRESENTATION(#17126,#17281);
#17075=SHAPE_DEFINITION_REPRESENTATION(#17127,#17282);
#17076=SHAPE_DEFINITION_REPRESENTATION(#17128,#17283);
#17077=SHAPE_DEFINITION_REPRESENTATION(#17129,#17284);
#17078=SHAPE_DEFINITION_REPRESENTATION(#17130,#17285);
#17079=SHAPE_DEFINITION_REPRESENTATION(#17131,#17286);
#17080=SHAPE_DEFINITION_REPRESENTATION(#17132,#17287);
#17081=SHAPE_DEFINITION_REPRESENTATION(#17133,#17288);
#17082=SHAPE_DEFINITION_REPRESENTATION(#17134,#17289);
#17083=SHAPE_DEFINITION_REPRESENTATION(#17140,#17290);
#17084=SHAPE_DEFINITION_REPRESENTATION(#17141,#17291);
#17085=SHAPE_DEFINITION_REPRESENTATION(#17142,#17292);
#17086=SHAPE_DEFINITION_REPRESENTATION(#17143,#17293);
#17087=SHAPE_DEFINITION_REPRESENTATION(#17144,#17294);
#17088=SHAPE_DEFINITION_REPRESENTATION(#17145,#17295);
#17089=SHAPE_DEFINITION_REPRESENTATION(#17146,#17296);
#17090=SHAPE_DEFINITION_REPRESENTATION(#17147,#17297);
#17091=SHAPE_DEFINITION_REPRESENTATION(#17148,#17298);
#17092=SHAPE_DEFINITION_REPRESENTATION(#17149,#17299);
#17093=SHAPE_DEFINITION_REPRESENTATION(#17150,#17300);
#17094=SHAPE_DEFINITION_REPRESENTATION(#17228,#17301);
#17095=SHAPE_DEFINITION_REPRESENTATION(#17229,#17302);
#17096=SHAPE_DEFINITION_REPRESENTATION(#17230,#17303);
#17097=SHAPE_DEFINITION_REPRESENTATION(#17231,#17304);
#17098=SHAPE_DEFINITION_REPRESENTATION(#17232,#17305);
#17099=SHAPE_DEFINITION_REPRESENTATION(#17233,#17306);
#17100=SHAPE_DEFINITION_REPRESENTATION(#17234,#17307);
#17101=SHAPE_DEFINITION_REPRESENTATION(#17235,#17308);
#17102=SHAPE_DEFINITION_REPRESENTATION(#17236,#17309);
#17103=PRODUCT_DEFINITION_SHAPE('',$,#17311);
#17104=PRODUCT_DEFINITION_SHAPE('',$,#17312);
#17105=PRODUCT_DEFINITION_SHAPE('',$,#17313);
#17106=PRODUCT_DEFINITION_SHAPE('',$,#17314);
#17107=PRODUCT_DEFINITION_SHAPE('',$,#17315);
#17108=PRODUCT_DEFINITION_SHAPE('',$,#17316);
#17109=PRODUCT_DEFINITION_SHAPE('',$,#17317);
#17110=PRODUCT_DEFINITION_SHAPE('',$,#17318);
#17111=PRODUCT_DEFINITION_SHAPE('',$,#17319);
#17112=PRODUCT_DEFINITION_SHAPE('',$,#17320);
#17113=PRODUCT_DEFINITION_SHAPE('',$,#17321);
#17114=PRODUCT_DEFINITION_SHAPE('',$,#17322);
#17115=PRODUCT_DEFINITION_SHAPE('',$,#17323);
#17116=PRODUCT_DEFINITION_SHAPE('',$,#17324);
#17117=PRODUCT_DEFINITION_SHAPE('',$,#17325);
#17118=PRODUCT_DEFINITION_SHAPE('',$,#17326);
#17119=PRODUCT_DEFINITION_SHAPE('',$,#17327);
#17120=PRODUCT_DEFINITION_SHAPE('',$,#17328);
#17121=PRODUCT_DEFINITION_SHAPE('',$,#17329);
#17122=PRODUCT_DEFINITION_SHAPE('',$,#17330);
#17123=PRODUCT_DEFINITION_SHAPE('',$,#17331);
#17124=PRODUCT_DEFINITION_SHAPE('',$,#17332);
#17125=PRODUCT_DEFINITION_SHAPE('',$,#17333);
#17126=PRODUCT_DEFINITION_SHAPE('',$,#17334);
#17127=PRODUCT_DEFINITION_SHAPE('',$,#17335);
#17128=PRODUCT_DEFINITION_SHAPE('',$,#17336);
#17129=PRODUCT_DEFINITION_SHAPE('',$,#17337);
#17130=PRODUCT_DEFINITION_SHAPE('',$,#17338);
#17131=PRODUCT_DEFINITION_SHAPE('',$,#17339);
#17132=PRODUCT_DEFINITION_SHAPE('',$,#17340);
#17133=PRODUCT_DEFINITION_SHAPE('',$,#17341);
#17134=PRODUCT_DEFINITION_SHAPE('',$,#17342);
#17135=PRODUCT_DEFINITION_SHAPE($,$,#332);
#17136=PRODUCT_DEFINITION_SHAPE($,$,#333);
#17137=PRODUCT_DEFINITION_SHAPE($,$,#334);
#17138=PRODUCT_DEFINITION_SHAPE($,$,#335);
#17139=PRODUCT_DEFINITION_SHAPE($,$,#336);
#17140=PRODUCT_DEFINITION_SHAPE('',$,#17343);
#17141=PRODUCT_DEFINITION_SHAPE('',$,#17344);
#17142=PRODUCT_DEFINITION_SHAPE('',$,#17345);
#17143=PRODUCT_DEFINITION_SHAPE('',$,#17346);
#17144=PRODUCT_DEFINITION_SHAPE('',$,#17347);
#17145=PRODUCT_DEFINITION_SHAPE('',$,#17348);
#17146=PRODUCT_DEFINITION_SHAPE('',$,#17349);
#17147=PRODUCT_DEFINITION_SHAPE('',$,#17350);
#17148=PRODUCT_DEFINITION_SHAPE('',$,#17351);
#17149=PRODUCT_DEFINITION_SHAPE('',$,#17352);
#17150=PRODUCT_DEFINITION_SHAPE('',$,#17353);
#17151=PRODUCT_DEFINITION_SHAPE($,$,#337);
#17152=PRODUCT_DEFINITION_SHAPE($,$,#338);
#17153=PRODUCT_DEFINITION_SHAPE($,$,#339);
#17154=PRODUCT_DEFINITION_SHAPE($,$,#340);
#17155=PRODUCT_DEFINITION_SHAPE($,$,#341);
#17156=PRODUCT_DEFINITION_SHAPE($,$,#342);
#17157=PRODUCT_DEFINITION_SHAPE($,$,#343);
#17158=PRODUCT_DEFINITION_SHAPE($,$,#344);
#17159=PRODUCT_DEFINITION_SHAPE($,$,#345);
#17160=PRODUCT_DEFINITION_SHAPE($,$,#346);
#17161=PRODUCT_DEFINITION_SHAPE($,$,#347);
#17162=PRODUCT_DEFINITION_SHAPE($,$,#348);
#17163=PRODUCT_DEFINITION_SHAPE($,$,#349);
#17164=PRODUCT_DEFINITION_SHAPE($,$,#350);
#17165=PRODUCT_DEFINITION_SHAPE($,$,#351);
#17166=PRODUCT_DEFINITION_SHAPE($,$,#352);
#17167=PRODUCT_DEFINITION_SHAPE($,$,#353);
#17168=PRODUCT_DEFINITION_SHAPE($,$,#354);
#17169=PRODUCT_DEFINITION_SHAPE($,$,#355);
#17170=PRODUCT_DEFINITION_SHAPE($,$,#356);
#17171=PRODUCT_DEFINITION_SHAPE($,$,#357);
#17172=PRODUCT_DEFINITION_SHAPE($,$,#358);
#17173=PRODUCT_DEFINITION_SHAPE($,$,#359);
#17174=PRODUCT_DEFINITION_SHAPE($,$,#360);
#17175=PRODUCT_DEFINITION_SHAPE($,$,#361);
#17176=PRODUCT_DEFINITION_SHAPE($,$,#362);
#17177=PRODUCT_DEFINITION_SHAPE($,$,#363);
#17178=PRODUCT_DEFINITION_SHAPE($,$,#364);
#17179=PRODUCT_DEFINITION_SHAPE($,$,#365);
#17180=PRODUCT_DEFINITION_SHAPE($,$,#366);
#17181=PRODUCT_DEFINITION_SHAPE($,$,#367);
#17182=PRODUCT_DEFINITION_SHAPE($,$,#368);
#17183=PRODUCT_DEFINITION_SHAPE($,$,#369);
#17184=PRODUCT_DEFINITION_SHAPE($,$,#370);
#17185=PRODUCT_DEFINITION_SHAPE($,$,#371);
#17186=PRODUCT_DEFINITION_SHAPE($,$,#372);
#17187=PRODUCT_DEFINITION_SHAPE($,$,#373);
#17188=PRODUCT_DEFINITION_SHAPE($,$,#374);
#17189=PRODUCT_DEFINITION_SHAPE($,$,#375);
#17190=PRODUCT_DEFINITION_SHAPE($,$,#376);
#17191=PRODUCT_DEFINITION_SHAPE($,$,#377);
#17192=PRODUCT_DEFINITION_SHAPE($,$,#378);
#17193=PRODUCT_DEFINITION_SHAPE($,$,#379);
#17194=PRODUCT_DEFINITION_SHAPE($,$,#380);
#17195=PRODUCT_DEFINITION_SHAPE($,$,#381);
#17196=PRODUCT_DEFINITION_SHAPE($,$,#382);
#17197=PRODUCT_DEFINITION_SHAPE($,$,#383);
#17198=PRODUCT_DEFINITION_SHAPE($,$,#384);
#17199=PRODUCT_DEFINITION_SHAPE($,$,#385);
#17200=PRODUCT_DEFINITION_SHAPE($,$,#386);
#17201=PRODUCT_DEFINITION_SHAPE($,$,#387);
#17202=PRODUCT_DEFINITION_SHAPE($,$,#388);
#17203=PRODUCT_DEFINITION_SHAPE($,$,#389);
#17204=PRODUCT_DEFINITION_SHAPE($,$,#390);
#17205=PRODUCT_DEFINITION_SHAPE($,$,#391);
#17206=PRODUCT_DEFINITION_SHAPE($,$,#392);
#17207=PRODUCT_DEFINITION_SHAPE($,$,#393);
#17208=PRODUCT_DEFINITION_SHAPE($,$,#394);
#17209=PRODUCT_DEFINITION_SHAPE($,$,#395);
#17210=PRODUCT_DEFINITION_SHAPE($,$,#396);
#17211=PRODUCT_DEFINITION_SHAPE($,$,#397);
#17212=PRODUCT_DEFINITION_SHAPE($,$,#398);
#17213=PRODUCT_DEFINITION_SHAPE($,$,#399);
#17214=PRODUCT_DEFINITION_SHAPE($,$,#400);
#17215=PRODUCT_DEFINITION_SHAPE($,$,#401);
#17216=PRODUCT_DEFINITION_SHAPE($,$,#402);
#17217=PRODUCT_DEFINITION_SHAPE($,$,#403);
#17218=PRODUCT_DEFINITION_SHAPE($,$,#404);
#17219=PRODUCT_DEFINITION_SHAPE($,$,#405);
#17220=PRODUCT_DEFINITION_SHAPE($,$,#406);
#17221=PRODUCT_DEFINITION_SHAPE($,$,#407);
#17222=PRODUCT_DEFINITION_SHAPE($,$,#408);
#17223=PRODUCT_DEFINITION_SHAPE($,$,#409);
#17224=PRODUCT_DEFINITION_SHAPE($,$,#410);
#17225=PRODUCT_DEFINITION_SHAPE($,$,#411);
#17226=PRODUCT_DEFINITION_SHAPE($,$,#412);
#17227=PRODUCT_DEFINITION_SHAPE($,$,#413);
#17228=PRODUCT_DEFINITION_SHAPE('',$,#17354);
#17229=PRODUCT_DEFINITION_SHAPE('',$,#17355);
#17230=PRODUCT_DEFINITION_SHAPE('',$,#17356);
#17231=PRODUCT_DEFINITION_SHAPE('',$,#17357);
#17232=PRODUCT_DEFINITION_SHAPE('',$,#17358);
#17233=PRODUCT_DEFINITION_SHAPE('',$,#17359);
#17234=PRODUCT_DEFINITION_SHAPE('',$,#17360);
#17235=PRODUCT_DEFINITION_SHAPE('',$,#17361);
#17236=PRODUCT_DEFINITION_SHAPE('',$,#17362);
#17237=PRODUCT_DEFINITION_SHAPE($,$,#414);
#17238=PRODUCT_DEFINITION_SHAPE($,$,#415);
#17239=PRODUCT_DEFINITION_SHAPE($,$,#416);
#17240=PRODUCT_DEFINITION_SHAPE($,$,#417);
#17241=PRODUCT_DEFINITION_SHAPE($,$,#418);
#17242=PRODUCT_DEFINITION_SHAPE($,$,#419);
#17243=PRODUCT_DEFINITION_SHAPE($,$,#420);
#17244=PRODUCT_DEFINITION_SHAPE($,$,#421);
#17245=PRODUCT_DEFINITION_SHAPE($,$,#422);
#17246=PRODUCT_DEFINITION_SHAPE($,$,#423);
#17247=PRODUCT_DEFINITION_SHAPE($,$,#424);
#17248=PRODUCT_DEFINITION_SHAPE($,$,#425);
#17249=PRODUCT_DEFINITION_SHAPE($,$,#426);
#17250=PRODUCT_DEFINITION_SHAPE($,$,#427);
#17251=PRODUCT_DEFINITION_SHAPE($,$,#428);
#17252=PRODUCT_DEFINITION_SHAPE($,$,#429);
#17253=PRODUCT_DEFINITION_SHAPE($,$,#430);
#17254=PRODUCT_DEFINITION_SHAPE($,$,#431);
#17255=PRODUCT_DEFINITION_SHAPE($,$,#432);
#17256=PRODUCT_DEFINITION_SHAPE($,$,#433);
#17257=PRODUCT_DEFINITION_SHAPE($,$,#434);
#17258=SHAPE_REPRESENTATION('',(#8742,#9770,#9771,#9772),#16994);
#17259=SHAPE_REPRESENTATION('',(#8743,#9565,#9566,#9567,#9568,#9569,#9570,
#9571,#9572,#9573,#9574,#9575,#9576,#9577,#9578,#9579,#9580,#9581,#9582,
#9583,#9584,#9585,#9586,#9587,#9588,#9589,#9590,#9591,#9592,#9593,#9594,
#9595,#9596,#9597,#9598,#9599,#9600,#9601,#9602,#9603,#9604,#9605,#9606,
#9607,#9608,#9609,#9610,#9611,#9612,#9613,#9614,#9615,#9616,#9617,#9618,
#9619,#9620,#9621,#9622,#9623,#9624,#9625,#9626,#9627,#9628,#9629,#9630,
#9631,#9632,#9633,#9634,#9635,#9636,#9637,#9638,#9639,#9640,#9641),#16995);
#17260=SHAPE_REPRESENTATION('',(#8744),#16996);
#17261=SHAPE_REPRESENTATION('',(#8781),#16997);
#17262=SHAPE_REPRESENTATION('',(#8788),#16998);
#17263=SHAPE_REPRESENTATION('',(#8795),#16999);
#17264=SHAPE_REPRESENTATION('',(#8846),#17000);
#17265=SHAPE_REPRESENTATION('',(#8878),#17001);
#17266=SHAPE_REPRESENTATION('',(#8903),#17002);
#17267=SHAPE_REPRESENTATION('',(#8928),#17003);
#17268=SHAPE_REPRESENTATION('',(#8960),#17004);
#17269=SHAPE_REPRESENTATION('',(#8985),#17005);
#17270=SHAPE_REPRESENTATION('',(#9010),#17006);
#17271=SHAPE_REPRESENTATION('',(#9042),#17007);
#17272=SHAPE_REPRESENTATION('',(#9067),#17008);
#17273=SHAPE_REPRESENTATION('',(#9092),#17009);
#17274=SHAPE_REPRESENTATION('',(#9124),#17010);
#17275=SHAPE_REPRESENTATION('',(#9149),#17011);
#17276=SHAPE_REPRESENTATION('',(#9174),#17012);
#17277=SHAPE_REPRESENTATION('',(#9201),#17013);
#17278=SHAPE_REPRESENTATION('',(#9207),#17014);
#17279=SHAPE_REPRESENTATION('',(#9213),#17015);
#17280=SHAPE_REPRESENTATION('',(#9218),#17016);
#17281=SHAPE_REPRESENTATION('',(#9224),#17017);
#17282=SHAPE_REPRESENTATION('',(#9230),#17018);
#17283=SHAPE_REPRESENTATION('',(#9235),#17019);
#17284=SHAPE_REPRESENTATION('',(#9261,#9384,#9385,#9386,#9387,#9388),#17020);
#17285=SHAPE_REPRESENTATION('',(#9262),#17021);
#17286=SHAPE_REPRESENTATION('',(#9282),#17022);
#17287=SHAPE_REPRESENTATION('',(#9302),#17023);
#17288=SHAPE_REPRESENTATION('',(#9317),#17024);
#17289=SHAPE_REPRESENTATION('',(#9367),#17025);
#17290=SHAPE_REPRESENTATION('',(#9389),#17026);
#17291=SHAPE_REPRESENTATION('',(#9413),#17027);
#17292=SHAPE_REPRESENTATION('',(#9439),#17028);
#17293=SHAPE_REPRESENTATION('',(#9455,#9752,#9753,#9754,#9755,#9756,#9757,
#9758,#9759,#9760),#17029);
#17294=SHAPE_REPRESENTATION('',(#9456),#17030);
#17295=SHAPE_REPRESENTATION('',(#9481),#17031);
#17296=SHAPE_REPRESENTATION('',(#9490),#17032);
#17297=SHAPE_REPRESENTATION('',(#9505),#17033);
#17298=SHAPE_REPRESENTATION('',(#9521),#17034);
#17299=SHAPE_REPRESENTATION('',(#9530),#17035);
#17300=SHAPE_REPRESENTATION('',(#9539),#17036);
#17301=SHAPE_REPRESENTATION('',(#9642,#9761,#9762,#9763,#9764,#9765,#9766,
#9767,#9768,#9769),#17037);
#17302=SHAPE_REPRESENTATION('',(#9643),#17038);
#17303=SHAPE_REPRESENTATION('',(#9664),#17039);
#17304=SHAPE_REPRESENTATION('',(#9680),#17040);
#17305=SHAPE_REPRESENTATION('',(#9689),#17041);
#17306=SHAPE_REPRESENTATION('',(#9698),#17042);
#17307=SHAPE_REPRESENTATION('',(#9712),#17043);
#17308=SHAPE_REPRESENTATION('',(#9726),#17044);
#17309=SHAPE_REPRESENTATION('',(#9737),#17045);
#17310=PRODUCT_DEFINITION_CONTEXT('part definition',#17468,'design');
#17311=PRODUCT_DEFINITION('PAT-123',
'PAT-123',#17363,#17310);
#17312=PRODUCT_DEFINITION('Frame and preload carriage',
'Frame and preload carriage',#17364,#17310);
#17313=PRODUCT_DEFINITION('Base','Base',#17365,#17310);
#17314=PRODUCT_DEFINITION('Foot strip','Foot strip',#17366,#17310);
#17315=PRODUCT_DEFINITION('Foot strip (1)','Foot strip (1)',#17367,#17310);
#17316=PRODUCT_DEFINITION('Preload deck','Preload deck',#17368,#17310);
#17317=PRODUCT_DEFINITION('Input bearing carrier',
'Input bearing carrier',#17369,#17310);
#17318=PRODUCT_DEFINITION('Bearing cap','Bearing cap',#17370,#17310);
#17319=PRODUCT_DEFINITION('Bearing cap (1)','Bearing cap (1)',#17371,#17310);
#17320=PRODUCT_DEFINITION('Input bearing carrier (1)',
'Input bearing carrier (1)',#17372,#17310);
#17321=PRODUCT_DEFINITION('Bearing cap (2)','Bearing cap (2)',#17373,#17310);
#17322=PRODUCT_DEFINITION('Bearing cap (3)','Bearing cap (3)',#17374,#17310);
#17323=PRODUCT_DEFINITION('Output bearing carrier',
'Output bearing carrier',#17375,#17310);
#17324=PRODUCT_DEFINITION('Bearing cap (4)','Bearing cap (4)',#17376,#17310);
#17325=PRODUCT_DEFINITION('Bearing cap (5)','Bearing cap (5)',#17377,#17310);
#17326=PRODUCT_DEFINITION('Output bearing carrier (1)',
'Output bearing carrier (1)',#17378,#17310);
#17327=PRODUCT_DEFINITION('Bearing cap (6)','Bearing cap (6)',#17379,#17310);
#17328=PRODUCT_DEFINITION('Bearing cap (7)','Bearing cap (7)',#17380,#17310);
#17329=PRODUCT_DEFINITION('Preload reaction wall',
'Preload reaction wall',#17381,#17310);
#17330=PRODUCT_DEFINITION('Front spring seat','Front spring seat',#17382,
#17310);
#17331=PRODUCT_DEFINITION('Rear spring shoe','Rear spring shoe',#17383,
#17310);
#17332=PRODUCT_DEFINITION('Preload spring','Preload spring',#17384,#17310);
#17333=PRODUCT_DEFINITION('Front spring seat (1)','Front spring seat (1)',
#17385,#17310);
#17334=PRODUCT_DEFINITION('Rear spring shoe (1)','Rear spring shoe (1)',#17386,
#17310);
#17335=PRODUCT_DEFINITION('Preload spring (1)','Preload spring (1)',#17387,
#17310);
#17336=PRODUCT_DEFINITION('Cap Screw - M5x20','Cap Screw - M5x20',#17388,
#17310);
#17337=PRODUCT_DEFINITION('Sealed Ball Bearing - 12 x 32 x 10 mm',
'Sealed Ball Bearing - 12 x 32 x 10 mm',#17389,#17310);
#17338=PRODUCT_DEFINITION('Inner ring','Inner ring',#17390,#17310);
#17339=PRODUCT_DEFINITION('Outer ring','Outer ring',#17391,#17310);
#17340=PRODUCT_DEFINITION('Balls','Balls',#17392,#17310);
#17341=PRODUCT_DEFINITION('Cage','Cage',#17393,#17310);
#17342=PRODUCT_DEFINITION('Seals 2RS','Seals 2RS',#17394,#17310);
#17343=PRODUCT_DEFINITION('M4x10 Cap Screw','M4x10 Cap Screw',#17395,#17310);
#17344=PRODUCT_DEFINITION('Cap Screw - M6x25','Cap Screw - M6x25',#17396,
#17310);
#17345=PRODUCT_DEFINITION('Hex Nut - M6','Hex Nut - M6',#17397,#17310);
#17346=PRODUCT_DEFINITION('Face disc input','Face disc input',#17398,#17310);
#17347=PRODUCT_DEFINITION('Input shaft','Input shaft',#17399,#17310);
#17348=PRODUCT_DEFINITION('Input inner spacer','Input inner spacer',#17400,
#17310);
#17349=PRODUCT_DEFINITION('Input rear collar','Input rear collar',#17401,
#17310);
#17350=PRODUCT_DEFINITION('Face disc','Face disc',#17402,#17310);
#17351=PRODUCT_DEFINITION('Friction face','Friction face',#17403,#17310);
#17352=PRODUCT_DEFINITION('Input keeper','Input keeper',#17404,#17310);
#17353=PRODUCT_DEFINITION('Cap Screw - M4x16','Cap Screw - M4x16',#17405,
#17310);
#17354=PRODUCT_DEFINITION('Rim wheel output','Rim wheel output',#17406,
#17310);
#17355=PRODUCT_DEFINITION('Output shaft','Output shaft',#17407,#17310);
#17356=PRODUCT_DEFINITION('Rim wheel','Rim wheel',#17408,#17310);
#17357=PRODUCT_DEFINITION('Friction rim band','Friction rim band',#17409,
#17310);
#17358=PRODUCT_DEFINITION('Output inner spacer','Output inner spacer',#17410,
#17310);
#17359=PRODUCT_DEFINITION('Output collar','Output collar',#17411,#17310);
#17360=PRODUCT_DEFINITION('Output collar (1)','Output collar (1)',#17412,
#17310);
#17361=PRODUCT_DEFINITION('Key 4x4x14','Key 4x4x14',#17413,#17310);
#17362=PRODUCT_DEFINITION('M5x5 collar screw','M5x5 collar screw',#17414,
#17310);
#17363=PRODUCT_DEFINITION_FORMATION('',$,#17470);
#17364=PRODUCT_DEFINITION_FORMATION('',$,#17471);
#17365=PRODUCT_DEFINITION_FORMATION('',$,#17472);
#17366=PRODUCT_DEFINITION_FORMATION('',$,#17473);
#17367=PRODUCT_DEFINITION_FORMATION('',$,#17474);
#17368=PRODUCT_DEFINITION_FORMATION('',$,#17475);
#17369=PRODUCT_DEFINITION_FORMATION('',$,#17476);
#17370=PRODUCT_DEFINITION_FORMATION('',$,#17477);
#17371=PRODUCT_DEFINITION_FORMATION('',$,#17478);
#17372=PRODUCT_DEFINITION_FORMATION('',$,#17479);
#17373=PRODUCT_DEFINITION_FORMATION('',$,#17480);
#17374=PRODUCT_DEFINITION_FORMATION('',$,#17481);
#17375=PRODUCT_DEFINITION_FORMATION('',$,#17482);
#17376=PRODUCT_DEFINITION_FORMATION('',$,#17483);
#17377=PRODUCT_DEFINITION_FORMATION('',$,#17484);
#17378=PRODUCT_DEFINITION_FORMATION('',$,#17485);
#17379=PRODUCT_DEFINITION_FORMATION('',$,#17486);
#17380=PRODUCT_DEFINITION_FORMATION('',$,#17487);
#17381=PRODUCT_DEFINITION_FORMATION('',$,#17488);
#17382=PRODUCT_DEFINITION_FORMATION('',$,#17489);
#17383=PRODUCT_DEFINITION_FORMATION('',$,#17490);
#17384=PRODUCT_DEFINITION_FORMATION('',$,#17491);
#17385=PRODUCT_DEFINITION_FORMATION('',$,#17492);
#17386=PRODUCT_DEFINITION_FORMATION('',$,#17493);
#17387=PRODUCT_DEFINITION_FORMATION('',$,#17494);
#17388=PRODUCT_DEFINITION_FORMATION('',$,#17495);
#17389=PRODUCT_DEFINITION_FORMATION('',$,#17496);
#17390=PRODUCT_DEFINITION_FORMATION('',$,#17497);
#17391=PRODUCT_DEFINITION_FORMATION('',$,#17498);
#17392=PRODUCT_DEFINITION_FORMATION('',$,#17499);
#17393=PRODUCT_DEFINITION_FORMATION('',$,#17500);
#17394=PRODUCT_DEFINITION_FORMATION('',$,#17501);
#17395=PRODUCT_DEFINITION_FORMATION('',$,#17502);
#17396=PRODUCT_DEFINITION_FORMATION('',$,#17503);
#17397=PRODUCT_DEFINITION_FORMATION('',$,#17504);
#17398=PRODUCT_DEFINITION_FORMATION('',$,#17505);
#17399=PRODUCT_DEFINITION_FORMATION('',$,#17506);
#17400=PRODUCT_DEFINITION_FORMATION('',$,#17507);
#17401=PRODUCT_DEFINITION_FORMATION('',$,#17508);
#17402=PRODUCT_DEFINITION_FORMATION('',$,#17509);
#17403=PRODUCT_DEFINITION_FORMATION('',$,#17510);
#17404=PRODUCT_DEFINITION_FORMATION('',$,#17511);
#17405=PRODUCT_DEFINITION_FORMATION('',$,#17512);
#17406=PRODUCT_DEFINITION_FORMATION('',$,#17513);
#17407=PRODUCT_DEFINITION_FORMATION('',$,#17514);
#17408=PRODUCT_DEFINITION_FORMATION('',$,#17515);
#17409=PRODUCT_DEFINITION_FORMATION('',$,#17516);
#17410=PRODUCT_DEFINITION_FORMATION('',$,#17517);
#17411=PRODUCT_DEFINITION_FORMATION('',$,#17518);
#17412=PRODUCT_DEFINITION_FORMATION('',$,#17519);
#17413=PRODUCT_DEFINITION_FORMATION('',$,#17520);
#17414=PRODUCT_DEFINITION_FORMATION('',$,#17521);
#17415=PRODUCT_RELATED_PRODUCT_CATEGORY('PAT-123','PAT-123',(#17470));
#17416=PRODUCT_RELATED_PRODUCT_CATEGORY('Frame and preload carriage',
'Frame and preload carriage',(#17471));
#17417=PRODUCT_RELATED_PRODUCT_CATEGORY('Base','Base',(#17472));
#17418=PRODUCT_RELATED_PRODUCT_CATEGORY('Foot strip','Foot strip',(#17473));
#17419=PRODUCT_RELATED_PRODUCT_CATEGORY('Foot strip (1)',
'Foot strip (1)',(#17474));
#17420=PRODUCT_RELATED_PRODUCT_CATEGORY('Preload deck','Preload deck',(#17475));
#17421=PRODUCT_RELATED_PRODUCT_CATEGORY('Input bearing carrier',
'Input bearing carrier',(#17476));
#17422=PRODUCT_RELATED_PRODUCT_CATEGORY('Bearing cap','Bearing cap',(#17477));
#17423=PRODUCT_RELATED_PRODUCT_CATEGORY('Bearing cap (1)',
'Bearing cap (1)',(#17478));
#17424=PRODUCT_RELATED_PRODUCT_CATEGORY('Input bearing carrier (1)',
'Input bearing carrier (1)',(#17479));
#17425=PRODUCT_RELATED_PRODUCT_CATEGORY('Bearing cap (2)',
'Bearing cap (2)',(#17480));
#17426=PRODUCT_RELATED_PRODUCT_CATEGORY('Bearing cap (3)',
'Bearing cap (3)',(#17481));
#17427=PRODUCT_RELATED_PRODUCT_CATEGORY('Output bearing carrier',
'Output bearing carrier',(#17482));
#17428=PRODUCT_RELATED_PRODUCT_CATEGORY('Bearing cap (4)',
'Bearing cap (4)',(#17483));
#17429=PRODUCT_RELATED_PRODUCT_CATEGORY('Bearing cap (5)',
'Bearing cap (5)',(#17484));
#17430=PRODUCT_RELATED_PRODUCT_CATEGORY('Output bearing carrier (1)',
'Output bearing carrier (1)',(#17485));
#17431=PRODUCT_RELATED_PRODUCT_CATEGORY('Bearing cap (6)',
'Bearing cap (6)',(#17486));
#17432=PRODUCT_RELATED_PRODUCT_CATEGORY('Bearing cap (7)',
'Bearing cap (7)',(#17487));
#17433=PRODUCT_RELATED_PRODUCT_CATEGORY('Preload reaction wall',
'Preload reaction wall',(#17488));
#17434=PRODUCT_RELATED_PRODUCT_CATEGORY('Front spring seat',
'Front spring seat',(#17489));
#17435=PRODUCT_RELATED_PRODUCT_CATEGORY('Rear spring shoe',
'Rear spring shoe',(#17490));
#17436=PRODUCT_RELATED_PRODUCT_CATEGORY('Preload spring',
'Preload spring',(#17491));
#17437=PRODUCT_RELATED_PRODUCT_CATEGORY('Front spring seat (1)',
'Front spring seat (1)',(#17492));
#17438=PRODUCT_RELATED_PRODUCT_CATEGORY('Rear spring shoe (1)',
'Rear spring shoe (1)',(#17493));
#17439=PRODUCT_RELATED_PRODUCT_CATEGORY('Preload spring (1)',
'Preload spring (1)',(#17494));
#17440=PRODUCT_RELATED_PRODUCT_CATEGORY('Cap Screw - M5x20',
'Cap Screw - M5x20',(#17495));
#17441=PRODUCT_RELATED_PRODUCT_CATEGORY(
'Sealed Ball Bearing - 12 x 32 x 10 mm',
'Sealed Ball Bearing - 12 x 32 x 10 mm',(#17496));
#17442=PRODUCT_RELATED_PRODUCT_CATEGORY('Inner ring','Inner ring',(#17497));
#17443=PRODUCT_RELATED_PRODUCT_CATEGORY('Outer ring','Outer ring',(#17498));
#17444=PRODUCT_RELATED_PRODUCT_CATEGORY('Balls','Balls',(#17499));
#17445=PRODUCT_RELATED_PRODUCT_CATEGORY('Cage','Cage',(#17500));
#17446=PRODUCT_RELATED_PRODUCT_CATEGORY('Seals 2RS','Seals 2RS',(#17501));
#17447=PRODUCT_RELATED_PRODUCT_CATEGORY('M4x10 Cap Screw',
'M4x10 Cap Screw',(#17502));
#17448=PRODUCT_RELATED_PRODUCT_CATEGORY('Cap Screw - M6x25',
'Cap Screw - M6x25',(#17503));
#17449=PRODUCT_RELATED_PRODUCT_CATEGORY('Hex Nut - M6','Hex Nut - M6',(#17504));
#17450=PRODUCT_RELATED_PRODUCT_CATEGORY('Face disc input',
'Face disc input',(#17505));
#17451=PRODUCT_RELATED_PRODUCT_CATEGORY('Input shaft','Input shaft',(#17506));
#17452=PRODUCT_RELATED_PRODUCT_CATEGORY('Input inner spacer',
'Input inner spacer',(#17507));
#17453=PRODUCT_RELATED_PRODUCT_CATEGORY('Input rear collar',
'Input rear collar',(#17508));
#17454=PRODUCT_RELATED_PRODUCT_CATEGORY('Face disc','Face disc',(#17509));
#17455=PRODUCT_RELATED_PRODUCT_CATEGORY('Friction face','Friction face',
(#17510));
#17456=PRODUCT_RELATED_PRODUCT_CATEGORY('Input keeper','Input keeper',(#17511));
#17457=PRODUCT_RELATED_PRODUCT_CATEGORY('Cap Screw - M4x16',
'Cap Screw - M4x16',(#17512));
#17458=PRODUCT_RELATED_PRODUCT_CATEGORY('Rim wheel output',
'Rim wheel output',(#17513));
#17459=PRODUCT_RELATED_PRODUCT_CATEGORY('Output shaft','Output shaft',(#17514));
#17460=PRODUCT_RELATED_PRODUCT_CATEGORY('Rim wheel','Rim wheel',(#17515));
#17461=PRODUCT_RELATED_PRODUCT_CATEGORY('Friction rim band',
'Friction rim band',(#17516));
#17462=PRODUCT_RELATED_PRODUCT_CATEGORY('Output inner spacer',
'Output inner spacer',(#17517));
#17463=PRODUCT_RELATED_PRODUCT_CATEGORY('Output collar','Output collar',
(#17518));
#17464=PRODUCT_RELATED_PRODUCT_CATEGORY('Output collar (1)',
'Output collar (1)',(#17519));
#17465=PRODUCT_RELATED_PRODUCT_CATEGORY('Key 4x4x14','Key 4x4x14',(#17520));
#17466=PRODUCT_RELATED_PRODUCT_CATEGORY('M5x5 collar screw',
'M5x5 collar screw',(#17521));
#17467=APPLICATION_PROTOCOL_DEFINITION('international standard',
'automotive_design',2009,#17468);
#17468=APPLICATION_CONTEXT(
'Core Data for Automotive Mechanical Design Process');
#17469=PRODUCT_CONTEXT('part definition',#17468,'mechanical');
#17470=PRODUCT('PAT-123','PAT-123',
'PAT-123',(#17469));
#17471=PRODUCT('Frame and preload carriage',
'Frame and preload carriage','Frame and preload carriage',(#17469));
#17472=PRODUCT('Base','Base','Base',(#17469));
#17473=PRODUCT('Foot strip','Foot strip','Foot strip',(#17469));
#17474=PRODUCT('Foot strip (1)','Foot strip (1)','Foot strip (1)',(#17469));
#17475=PRODUCT('Preload deck','Preload deck','Preload deck',(#17469));
#17476=PRODUCT('Input bearing carrier','Input bearing carrier',
'Input bearing carrier',(#17469));
#17477=PRODUCT('Bearing cap','Bearing cap','Bearing cap',(#17469));
#17478=PRODUCT('Bearing cap (1)','Bearing cap (1)','Bearing cap (1)',(#17469));
#17479=PRODUCT('Input bearing carrier (1)','Input bearing carrier (1)',
'Input bearing carrier (1)',(#17469));
#17480=PRODUCT('Bearing cap (2)','Bearing cap (2)','Bearing cap (2)',(#17469));
#17481=PRODUCT('Bearing cap (3)','Bearing cap (3)','Bearing cap (3)',(#17469));
#17482=PRODUCT('Output bearing carrier','Output bearing carrier',
'Output bearing carrier',(#17469));
#17483=PRODUCT('Bearing cap (4)','Bearing cap (4)','Bearing cap (4)',(#17469));
#17484=PRODUCT('Bearing cap (5)','Bearing cap (5)','Bearing cap (5)',(#17469));
#17485=PRODUCT('Output bearing carrier (1)','Output bearing carrier (1)',
'Output bearing carrier (1)',(#17469));
#17486=PRODUCT('Bearing cap (6)','Bearing cap (6)','Bearing cap (6)',(#17469));
#17487=PRODUCT('Bearing cap (7)','Bearing cap (7)','Bearing cap (7)',(#17469));
#17488=PRODUCT('Preload reaction wall','Preload reaction wall',
'Preload reaction wall',(#17469));
#17489=PRODUCT('Front spring seat','Front spring seat',
'Front spring seat',(#17469));
#17490=PRODUCT('Rear spring shoe','Rear spring shoe','Rear spring shoe',
(#17469));
#17491=PRODUCT('Preload spring','Preload spring','Preload spring',(#17469));
#17492=PRODUCT('Front spring seat (1)','Front spring seat (1)',
'Front spring seat (1)',(#17469));
#17493=PRODUCT('Rear spring shoe (1)','Rear spring shoe (1)',
'Rear spring shoe (1)',(#17469));
#17494=PRODUCT('Preload spring (1)','Preload spring (1)','Preload spring (1)',
(#17469));
#17495=PRODUCT('Cap Screw - M5x20','Cap Screw - M5x20',
'Cap Screw - M5x20',(#17469));
#17496=PRODUCT('Sealed Ball Bearing - 12 x 32 x 10 mm',
'Sealed Ball Bearing - 12 x 32 x 10 mm',
'Sealed Ball Bearing - 12 x 32 x 10 mm',(#17469));
#17497=PRODUCT('Inner ring','Inner ring','Inner ring',(#17469));
#17498=PRODUCT('Outer ring','Outer ring','Outer ring',(#17469));
#17499=PRODUCT('Balls','Balls','Balls',(#17469));
#17500=PRODUCT('Cage','Cage','Cage',(#17469));
#17501=PRODUCT('Seals 2RS','Seals 2RS','Seals 2RS',(#17469));
#17502=PRODUCT('M4x10 Cap Screw','M4x10 Cap Screw','M4x10 Cap Screw',(#17469));
#17503=PRODUCT('Cap Screw - M6x25','Cap Screw - M6x25',
'Cap Screw - M6x25',(#17469));
#17504=PRODUCT('Hex Nut - M6','Hex Nut - M6','Hex Nut - M6',(#17469));
#17505=PRODUCT('Face disc input','Face disc input','Face disc input',(#17469));
#17506=PRODUCT('Input shaft','Input shaft','Input shaft',(#17469));
#17507=PRODUCT('Input inner spacer','Input inner spacer',
'Input inner spacer',(#17469));
#17508=PRODUCT('Input rear collar','Input rear collar',
'Input rear collar',(#17469));
#17509=PRODUCT('Face disc','Face disc','Face disc',(#17469));
#17510=PRODUCT('Friction face','Friction face','Friction face',(#17469));
#17511=PRODUCT('Input keeper','Input keeper','Input keeper',(#17469));
#17512=PRODUCT('Cap Screw - M4x16','Cap Screw - M4x16',
'Cap Screw - M4x16',(#17469));
#17513=PRODUCT('Rim wheel output','Rim wheel output','Rim wheel output',
(#17469));
#17514=PRODUCT('Output shaft','Output shaft','Output shaft',(#17469));
#17515=PRODUCT('Rim wheel','Rim wheel','Rim wheel',(#17469));
#17516=PRODUCT('Friction rim band','Friction rim band',
'Friction rim band',(#17469));
#17517=PRODUCT('Output inner spacer','Output inner spacer',
'Output inner spacer',(#17469));
#17518=PRODUCT('Output collar','Output collar','Output collar',(#17469));
#17519=PRODUCT('Output collar (1)','Output collar (1)','Output collar (1)',(#17469));
#17520=PRODUCT('Key 4x4x14','Key 4x4x14','Key 4x4x14',(#17469));
#17521=PRODUCT('M5x5 collar screw','M5x5 collar screw',
'M5x5 collar screw',(#17469));
#17522=PRESENTATION_STYLE_ASSIGNMENT((#17528));
#17523=PRESENTATION_STYLE_ASSIGNMENT((#17529));
#17524=PRESENTATION_STYLE_ASSIGNMENT((#17530));
#17525=PRESENTATION_STYLE_ASSIGNMENT((#17531));
#17526=PRESENTATION_STYLE_ASSIGNMENT((#17532));
#17527=PRESENTATION_STYLE_ASSIGNMENT((#17533));
#17528=SURFACE_STYLE_USAGE(.BOTH.,#17534);
#17529=SURFACE_STYLE_USAGE(.BOTH.,#17535);
#17530=SURFACE_STYLE_USAGE(.BOTH.,#17536);
#17531=SURFACE_STYLE_USAGE(.BOTH.,#17537);
#17532=SURFACE_STYLE_USAGE(.BOTH.,#17538);
#17533=SURFACE_STYLE_USAGE(.BOTH.,#17539);
#17534=SURFACE_SIDE_STYLE('',(#17540));
#17535=SURFACE_SIDE_STYLE('',(#17541));
#17536=SURFACE_SIDE_STYLE('',(#17542));
#17537=SURFACE_SIDE_STYLE('',(#17543));
#17538=SURFACE_SIDE_STYLE('',(#17544));
#17539=SURFACE_SIDE_STYLE('',(#17545));
#17540=SURFACE_STYLE_FILL_AREA(#17546);
#17541=SURFACE_STYLE_FILL_AREA(#17547);
#17542=SURFACE_STYLE_FILL_AREA(#17548);
#17543=SURFACE_STYLE_FILL_AREA(#17549);
#17544=SURFACE_STYLE_FILL_AREA(#17550);
#17545=SURFACE_STYLE_FILL_AREA(#17551);
#17546=FILL_AREA_STYLE('Steel - Satin',(#17552));
#17547=FILL_AREA_STYLE('CAD Library Painted - Deep blue',(#17553));
#17548=FILL_AREA_STYLE('CAD Library Painted - Engineering blue',(#17554));
#17549=FILL_AREA_STYLE('CAD Library Painted - Steel gray',(#17555));
#17550=FILL_AREA_STYLE('CAD Library Painted - Graphite',(#17556));
#17551=FILL_AREA_STYLE('CAD Library Painted - Light blue',(#17557));
#17552=FILL_AREA_STYLE_COLOUR('Steel - Satin',#17558);
#17553=FILL_AREA_STYLE_COLOUR('CAD Library Painted - Deep blue',#17559);
#17554=FILL_AREA_STYLE_COLOUR('CAD Library Painted - Engineering blue',
#17560);
#17555=FILL_AREA_STYLE_COLOUR('CAD Library Painted - Steel gray',#17561);
#17556=FILL_AREA_STYLE_COLOUR('CAD Library Painted - Graphite',#17562);
#17557=FILL_AREA_STYLE_COLOUR('CAD Library Painted - Light blue',#17563);
#17558=COLOUR_RGB('Steel - Satin',0.627450980392157,0.627450980392157,0.627450980392157);
#17559=COLOUR_RGB('CAD Library Painted - Deep blue',0.0784313725490196,
0.203921568627451,0.349019607843137);
#17560=COLOUR_RGB('CAD Library Painted - Engineering blue',0.12156862745098,
0.356862745098039,0.6);
#17561=COLOUR_RGB('CAD Library Painted - Steel gray',0.592156862745098,
0.631372549019608,0.67843137254902);
#17562=COLOUR_RGB('CAD Library Painted - Graphite',0.168627450980392,0.192156862745098,
0.231372549019608);
#17563=COLOUR_RGB('CAD Library Painted - Light blue',0.286274509803922,
0.552941176470588,0.780392156862745);
#17564=COLOUR_RGB('Dark Blue',0.08,0.2,0.34);
#17565=FILL_AREA_STYLE_COLOUR('',#17564);
#17566=FILL_AREA_STYLE('',(#17565));
#17567=SURFACE_STYLE_FILL_AREA(#17566);
#17568=SURFACE_SIDE_STYLE('',(#17567));
#17569=SURFACE_STYLE_USAGE(.BOTH.,#17568);
#17570=PRESENTATION_STYLE_ASSIGNMENT((#17569));
#17571=COLOUR_RGB('Light Blue',0.38,0.62,0.78);
#17572=FILL_AREA_STYLE_COLOUR('',#17571);
#17573=FILL_AREA_STYLE('',(#17572));
#17574=SURFACE_STYLE_FILL_AREA(#17573);
#17575=SURFACE_SIDE_STYLE('',(#17574));
#17576=SURFACE_STYLE_USAGE(.BOTH.,#17575);
#17577=PRESENTATION_STYLE_ASSIGNMENT((#17576));
#17578=COLOUR_RGB('Sky Blue',0.24,0.69,0.87);
#17579=FILL_AREA_STYLE_COLOUR('',#17578);
#17580=FILL_AREA_STYLE('',(#17579));
#17581=SURFACE_STYLE_FILL_AREA(#17580);
#17582=SURFACE_SIDE_STYLE('',(#17581));
#17583=SURFACE_STYLE_USAGE(.BOTH.,#17582);
#17584=PRESENTATION_STYLE_ASSIGNMENT((#17583));
#17585=COLOUR_RGB('Grey',0.48,0.52,0.57);
#17586=FILL_AREA_STYLE_COLOUR('',#17585);
#17587=FILL_AREA_STYLE('',(#17586));
#17588=SURFACE_STYLE_FILL_AREA(#17587);
#17589=SURFACE_SIDE_STYLE('',(#17588));
#17590=SURFACE_STYLE_USAGE(.BOTH.,#17589);
#17591=PRESENTATION_STYLE_ASSIGNMENT((#17590));
#17592=COLOUR_RGB('Black',0.12,0.14,0.17);
#17593=FILL_AREA_STYLE_COLOUR('',#17592);
#17594=FILL_AREA_STYLE('',(#17593));
#17595=SURFACE_STYLE_FILL_AREA(#17594);
#17596=SURFACE_SIDE_STYLE('',(#17595));
#17597=SURFACE_STYLE_USAGE(.BOTH.,#17596);
#17598=PRESENTATION_STYLE_ASSIGNMENT((#17597));
#17599=COLOUR_RGB('Off White',0.89,0.88,0.83);
#17600=FILL_AREA_STYLE_COLOUR('',#17599);
#17601=FILL_AREA_STYLE('',(#17600));
#17602=SURFACE_STYLE_FILL_AREA(#17601);
#17603=SURFACE_SIDE_STYLE('',(#17602));
#17604=SURFACE_STYLE_USAGE(.BOTH.,#17603);
#17605=PRESENTATION_STYLE_ASSIGNMENT((#17604));
ENDSEC;
END-ISO-10303-21;
